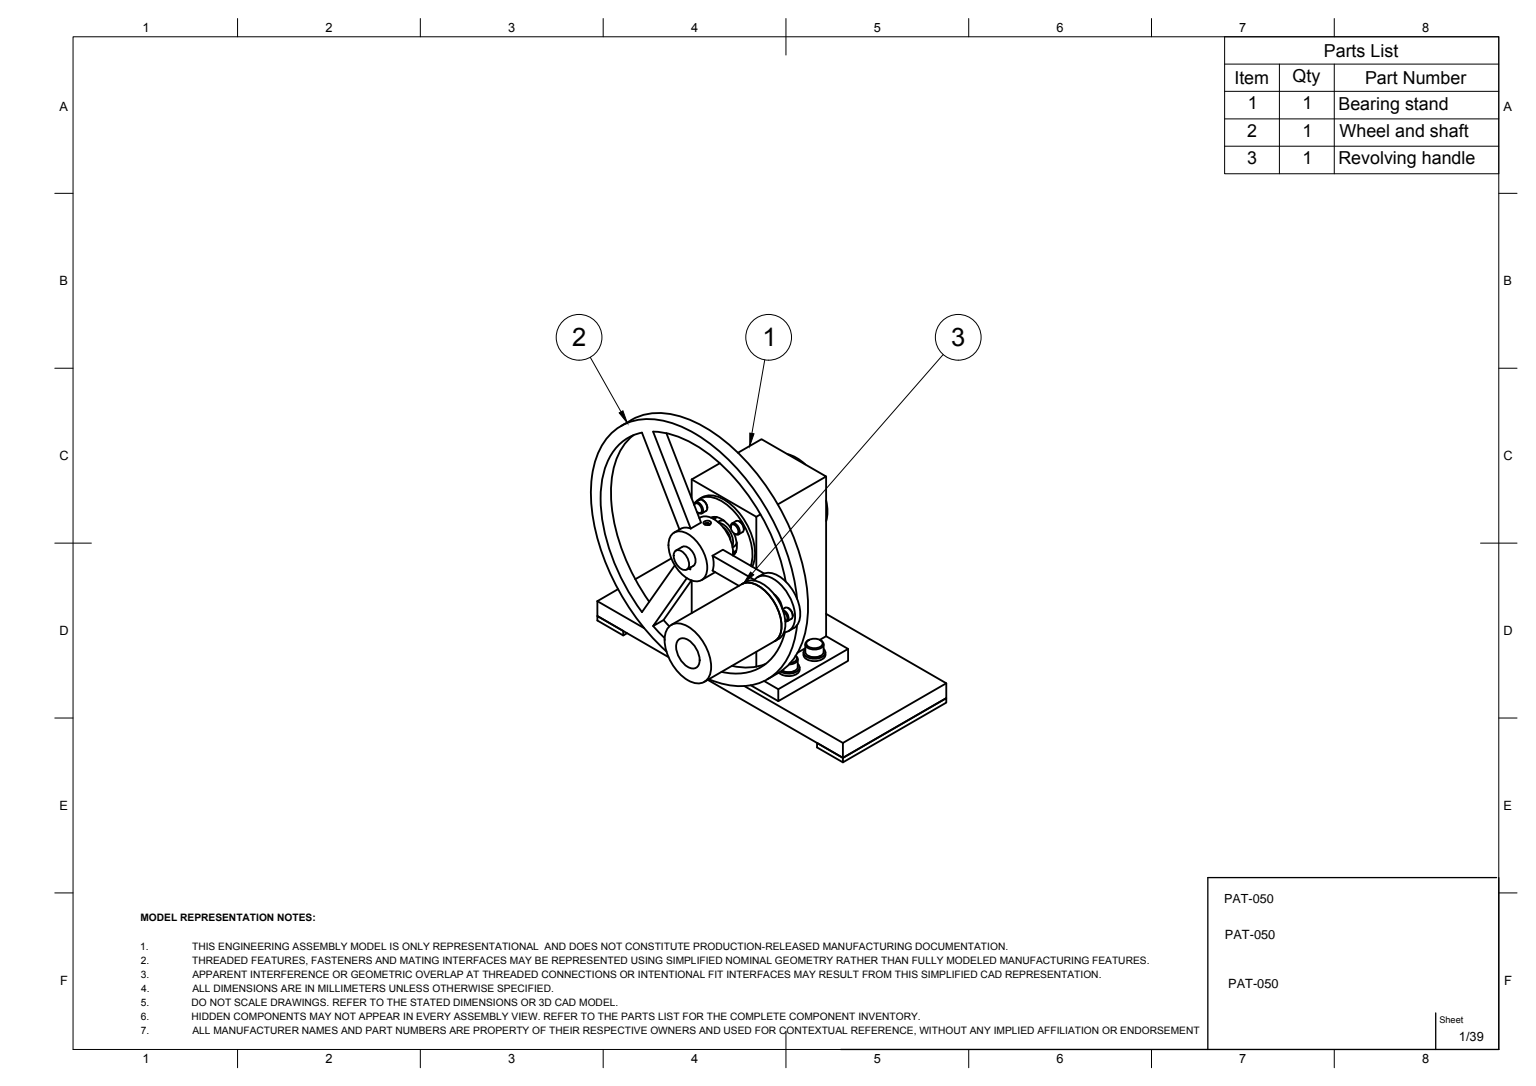
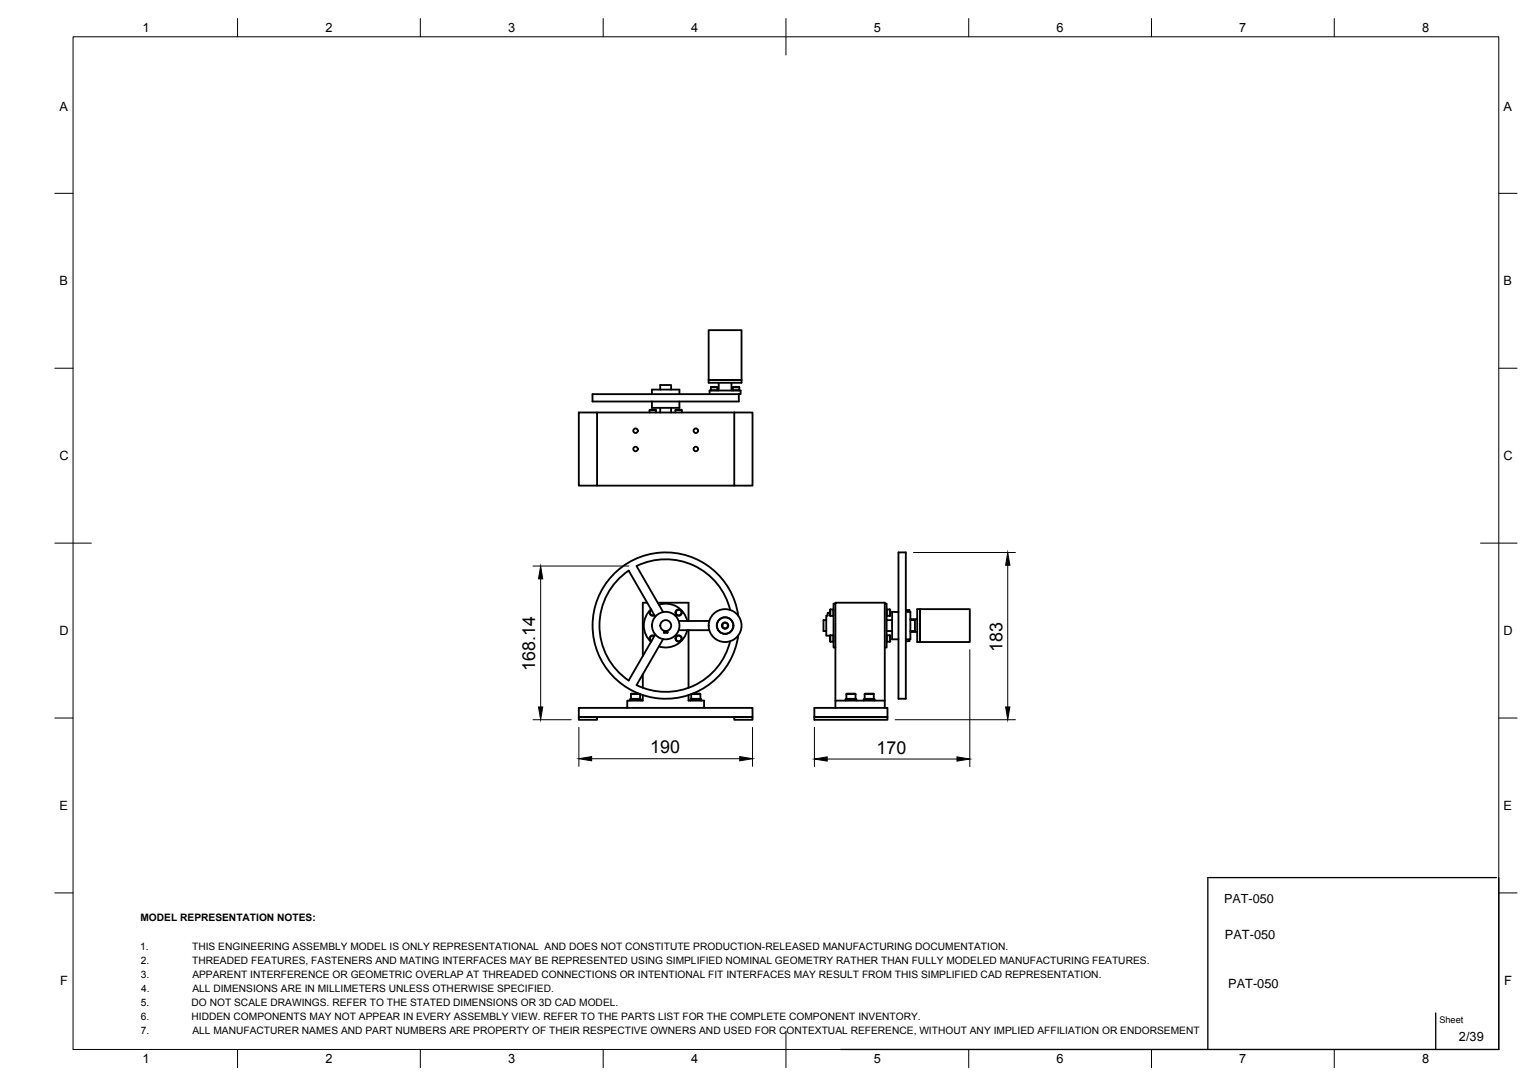
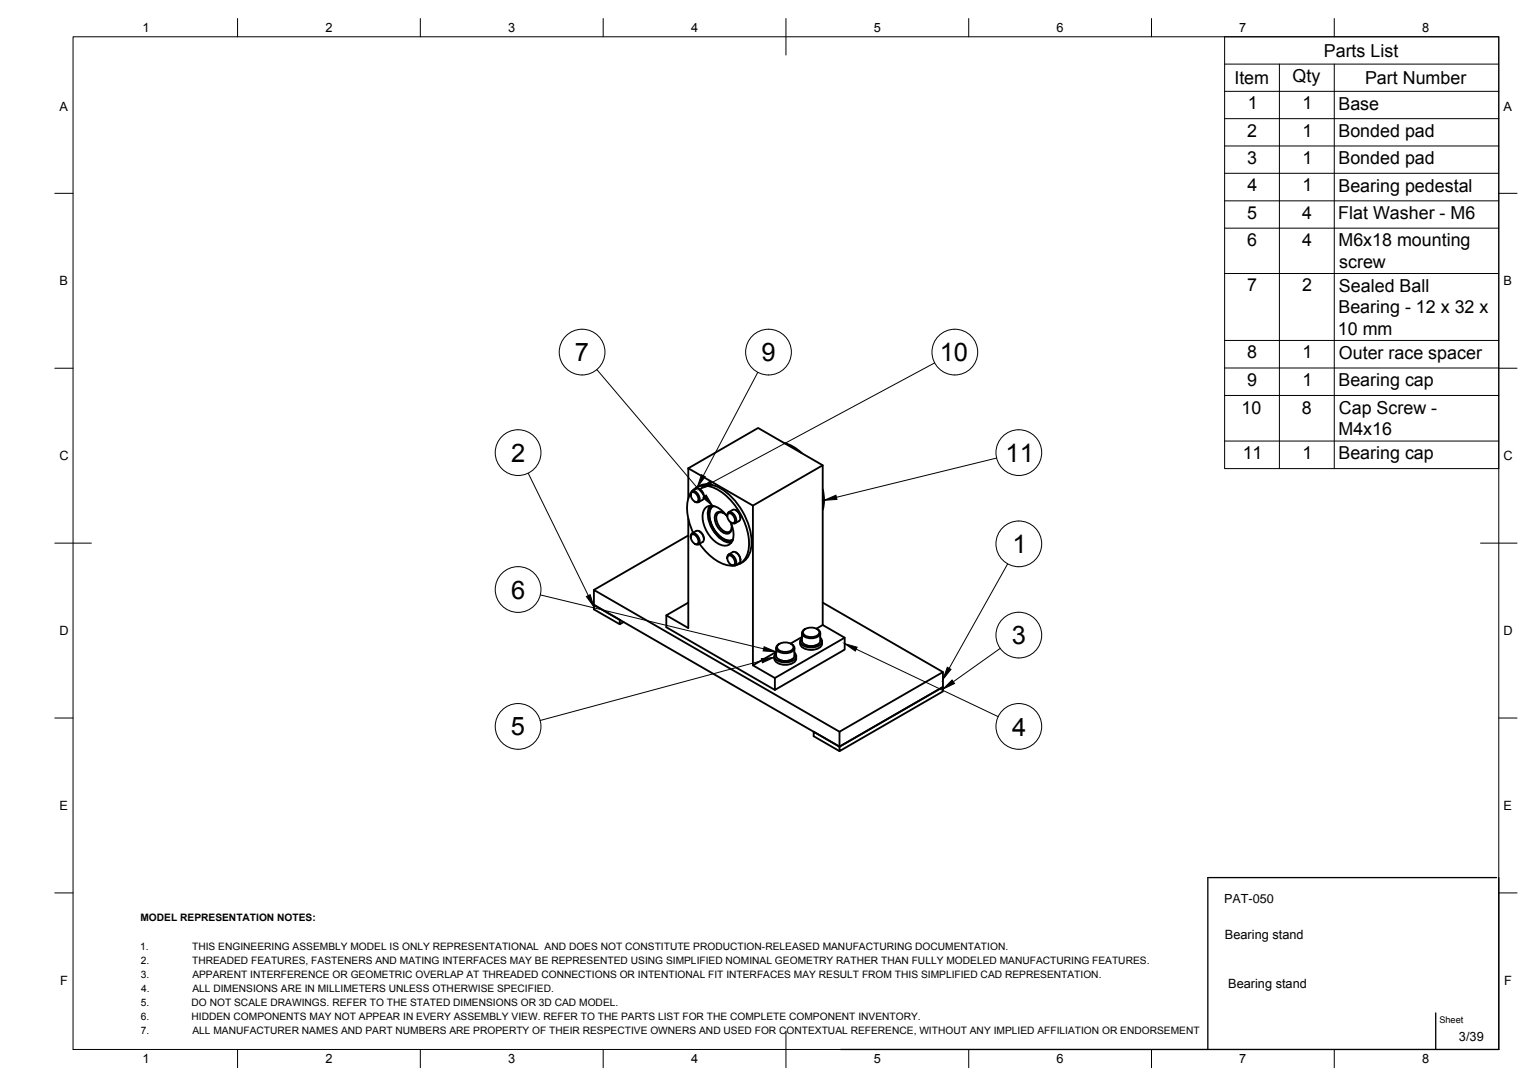
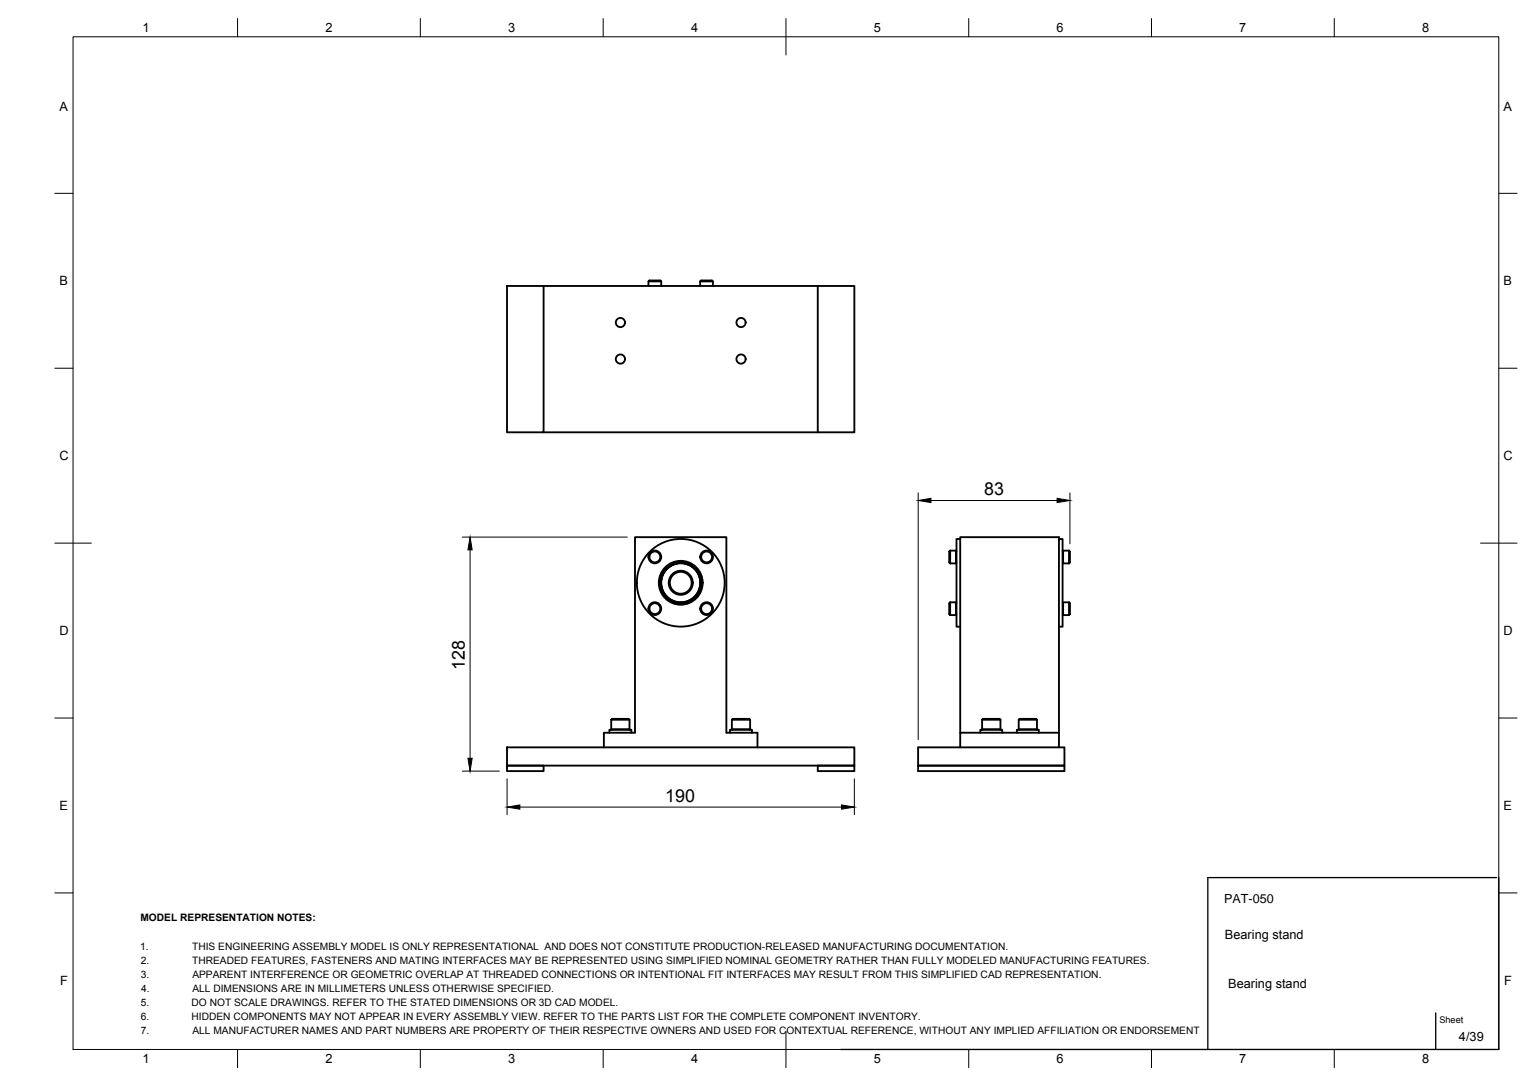
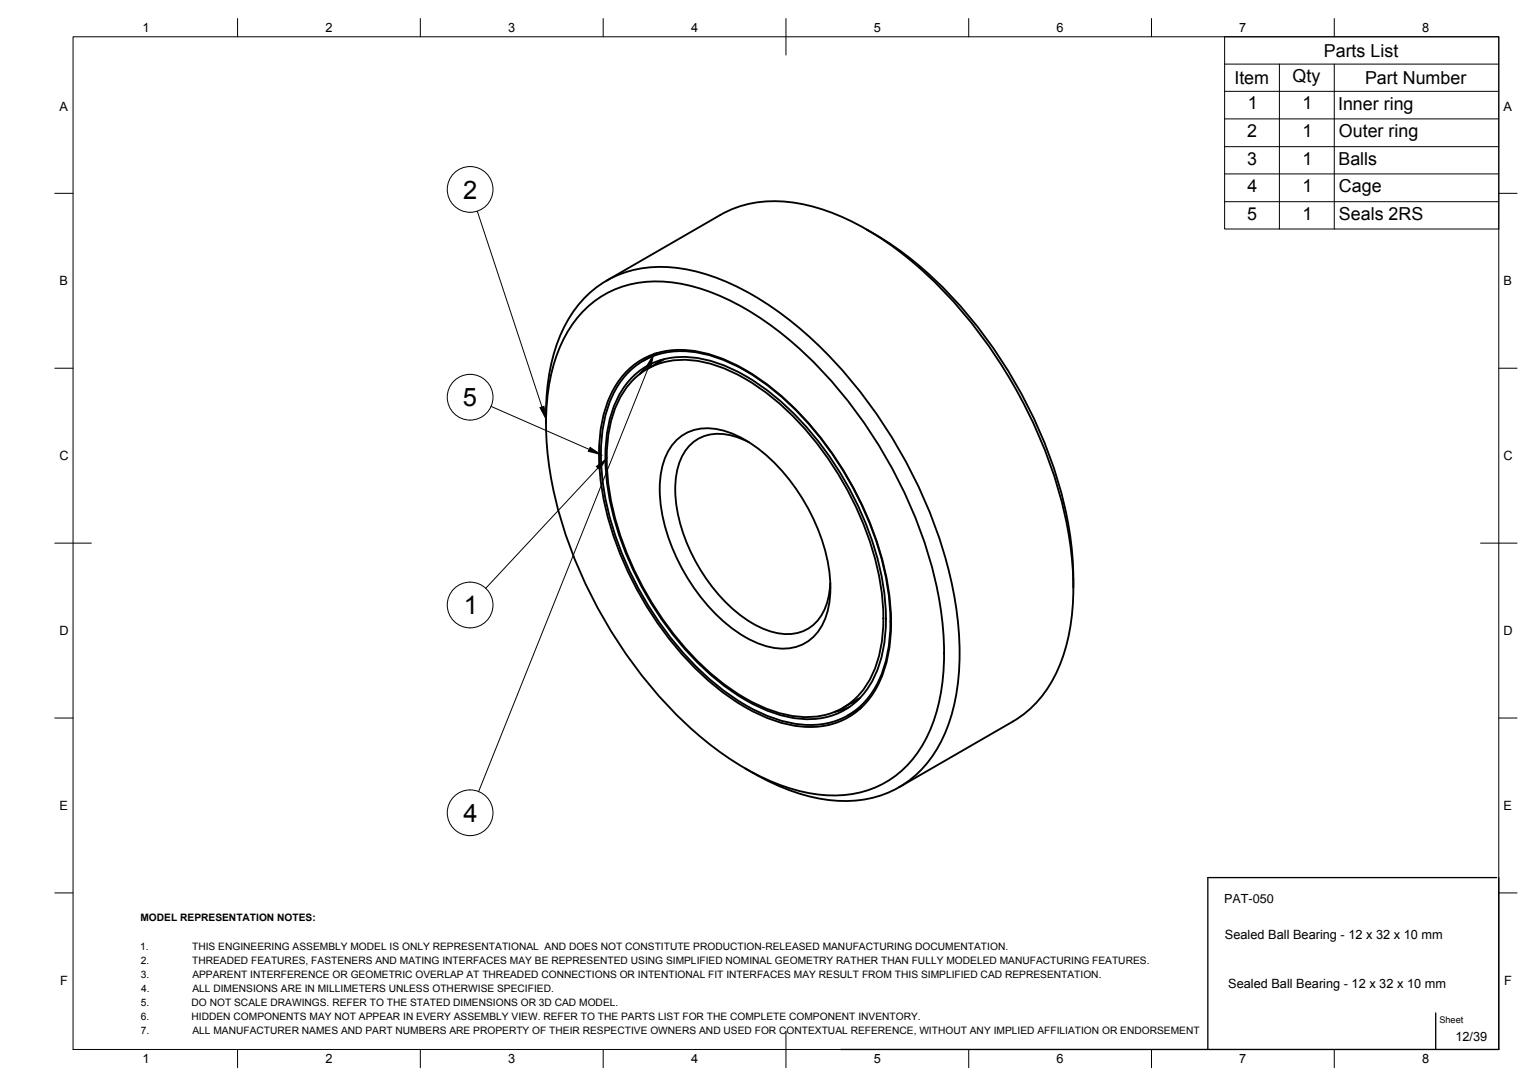
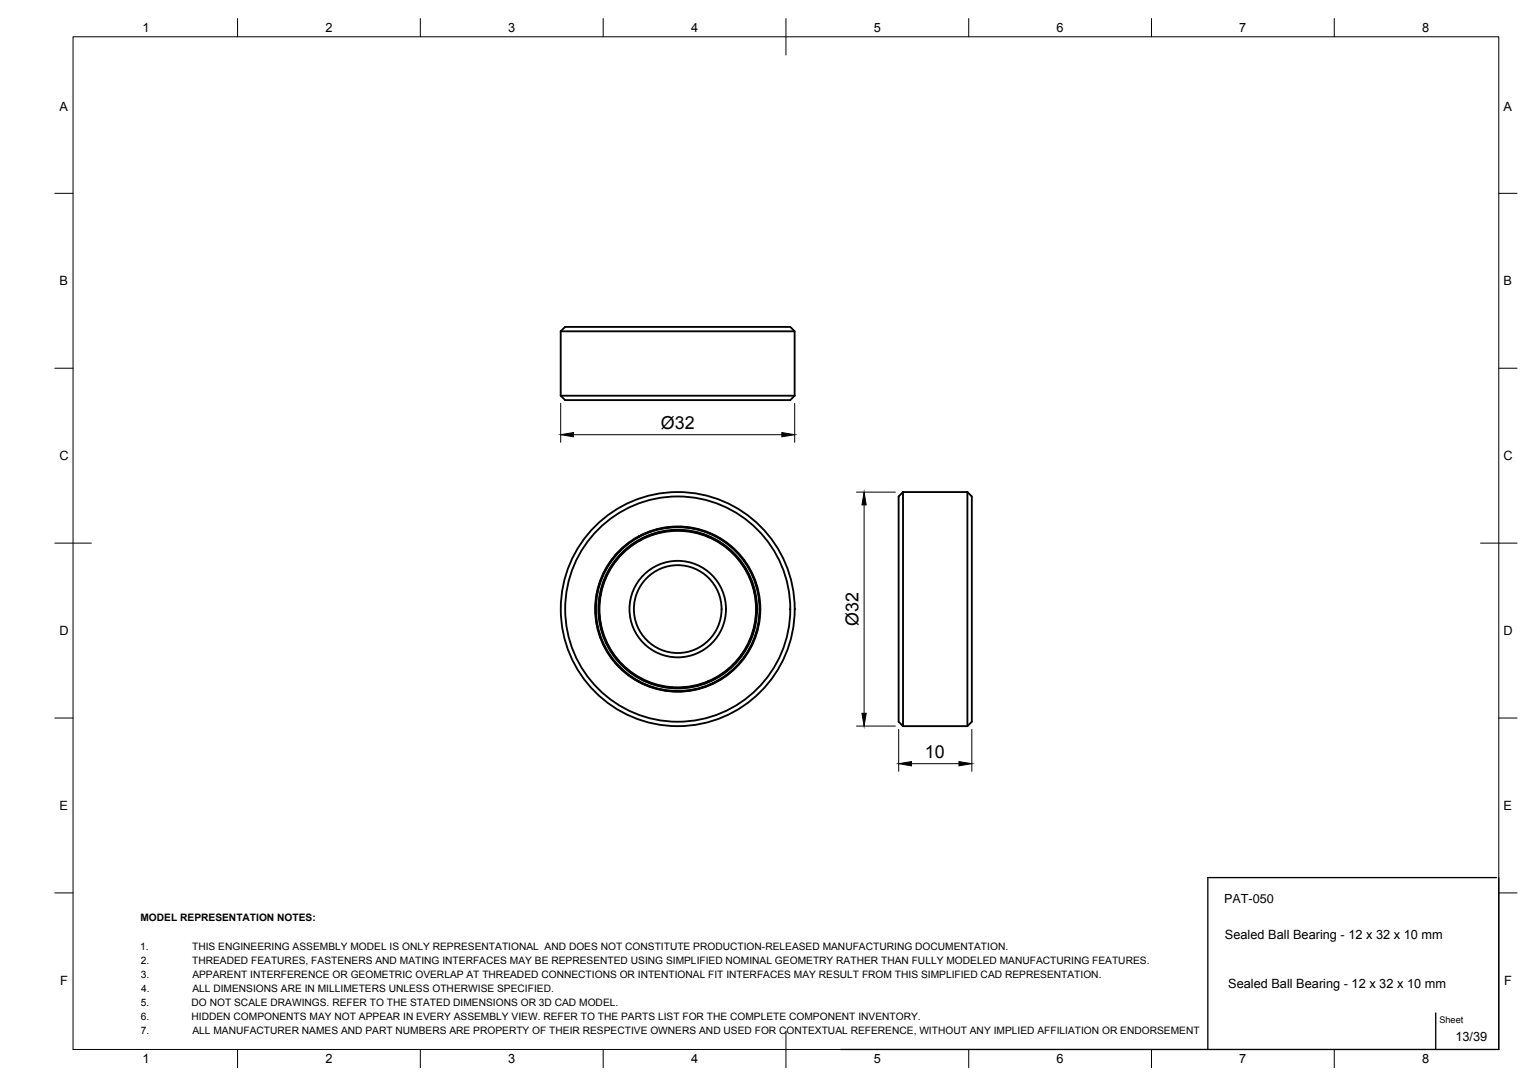
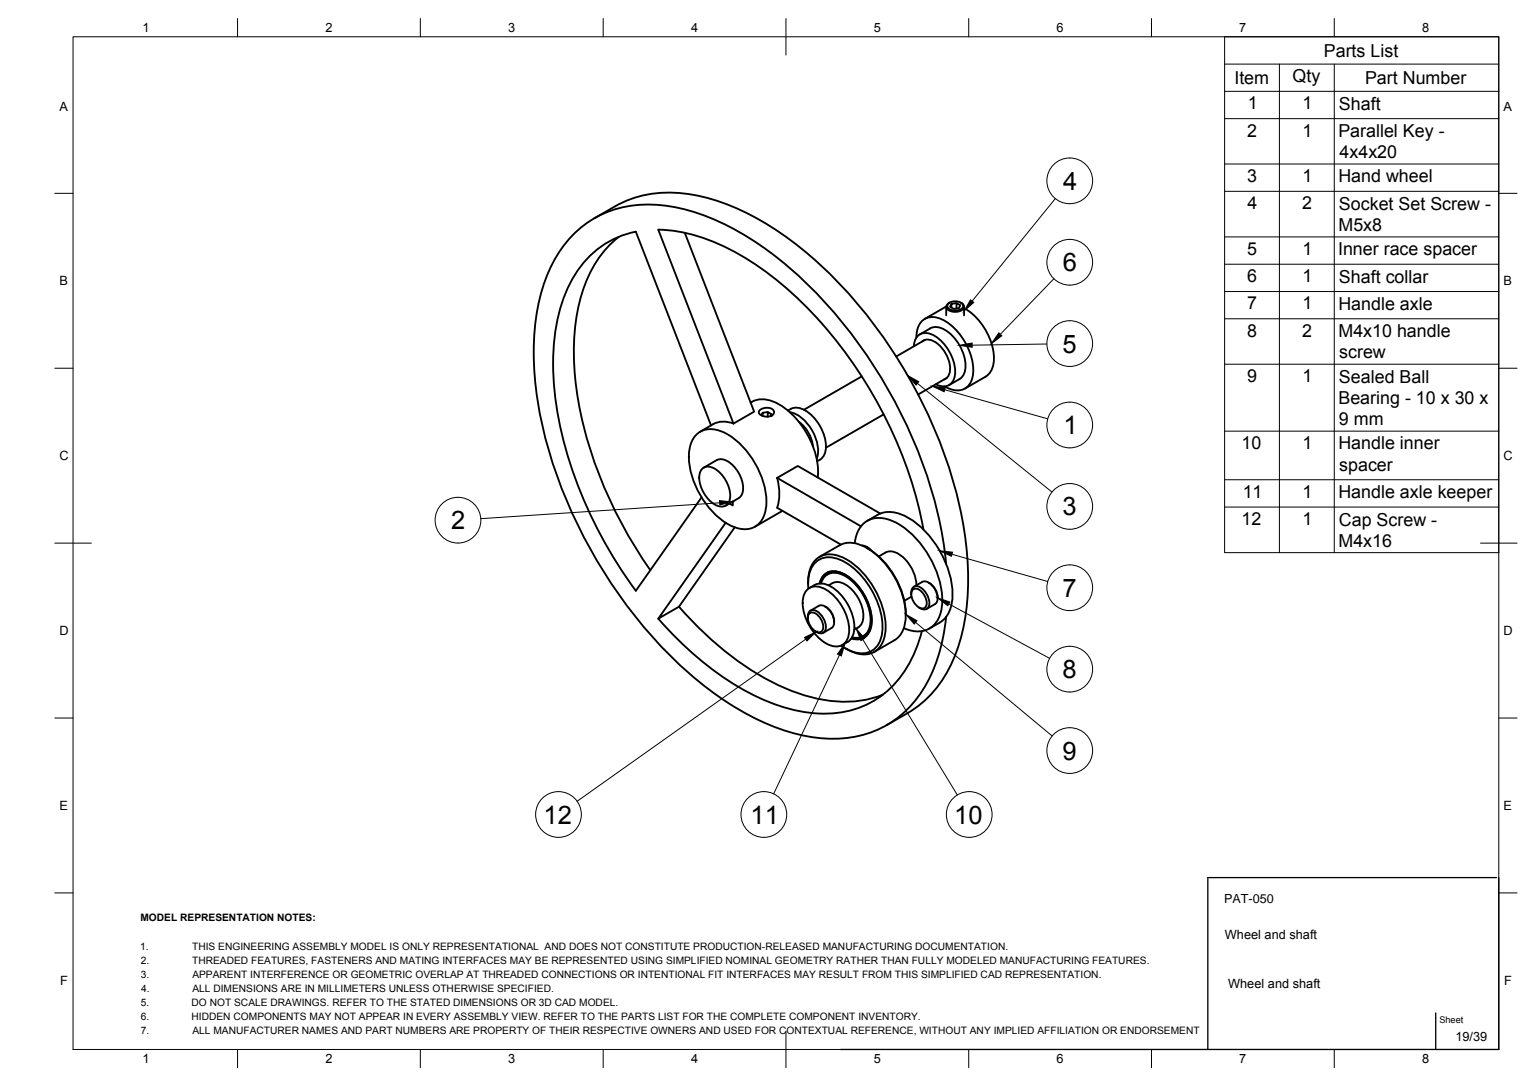
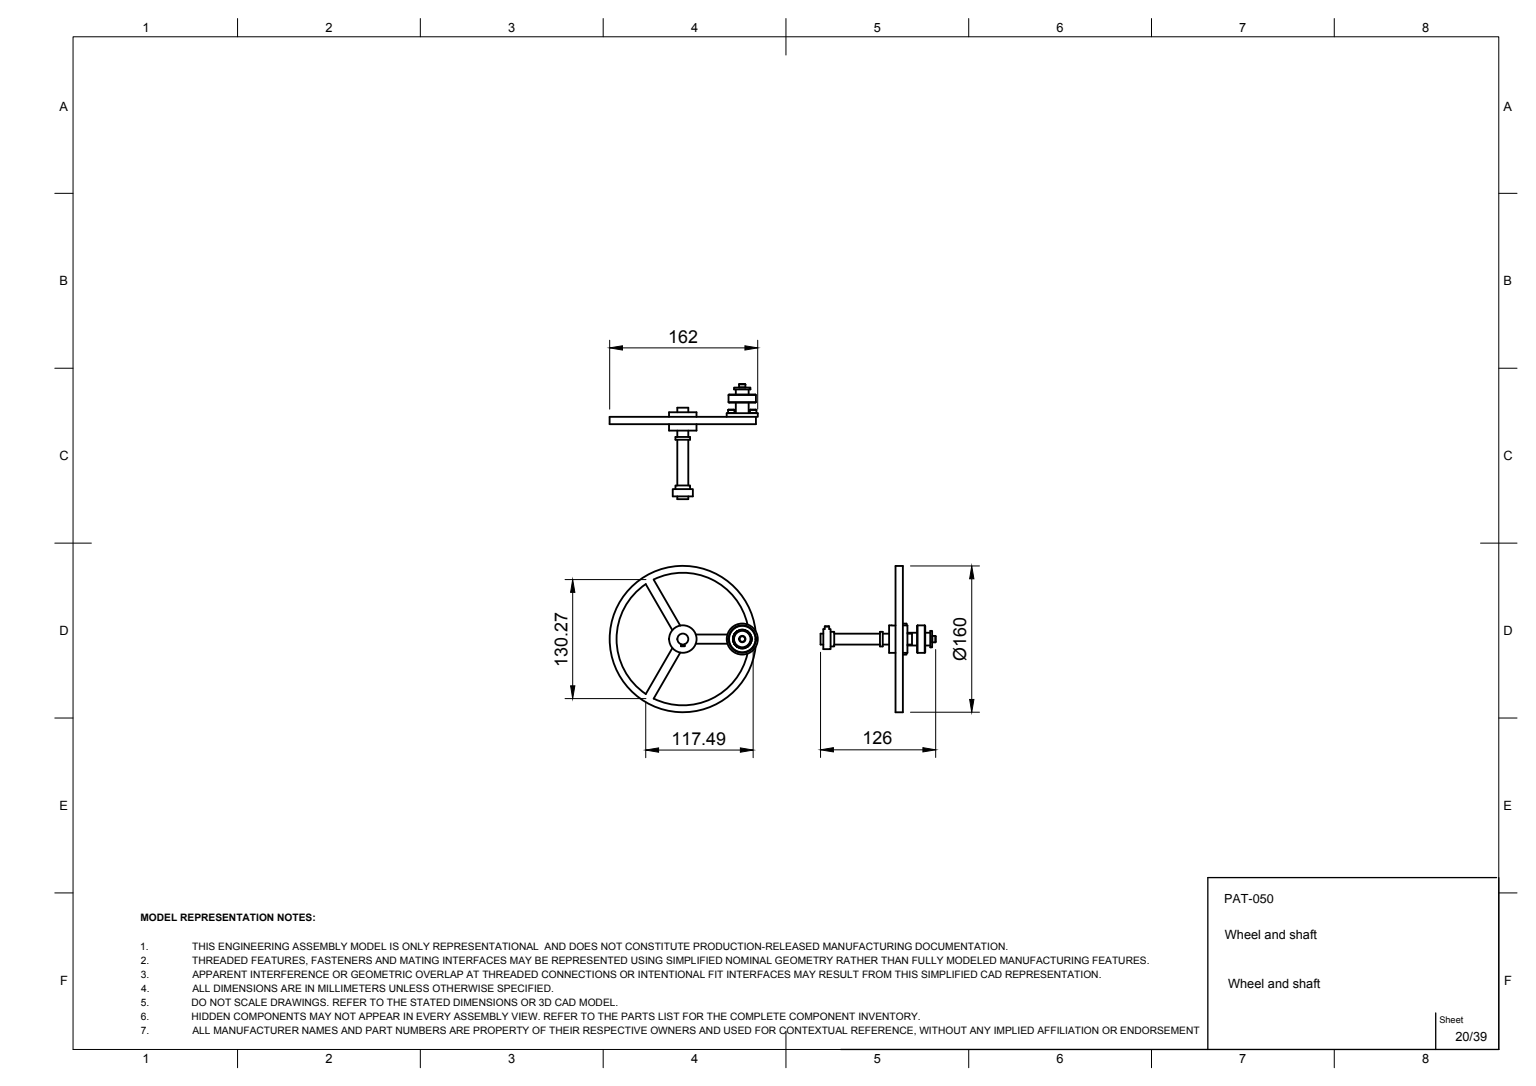
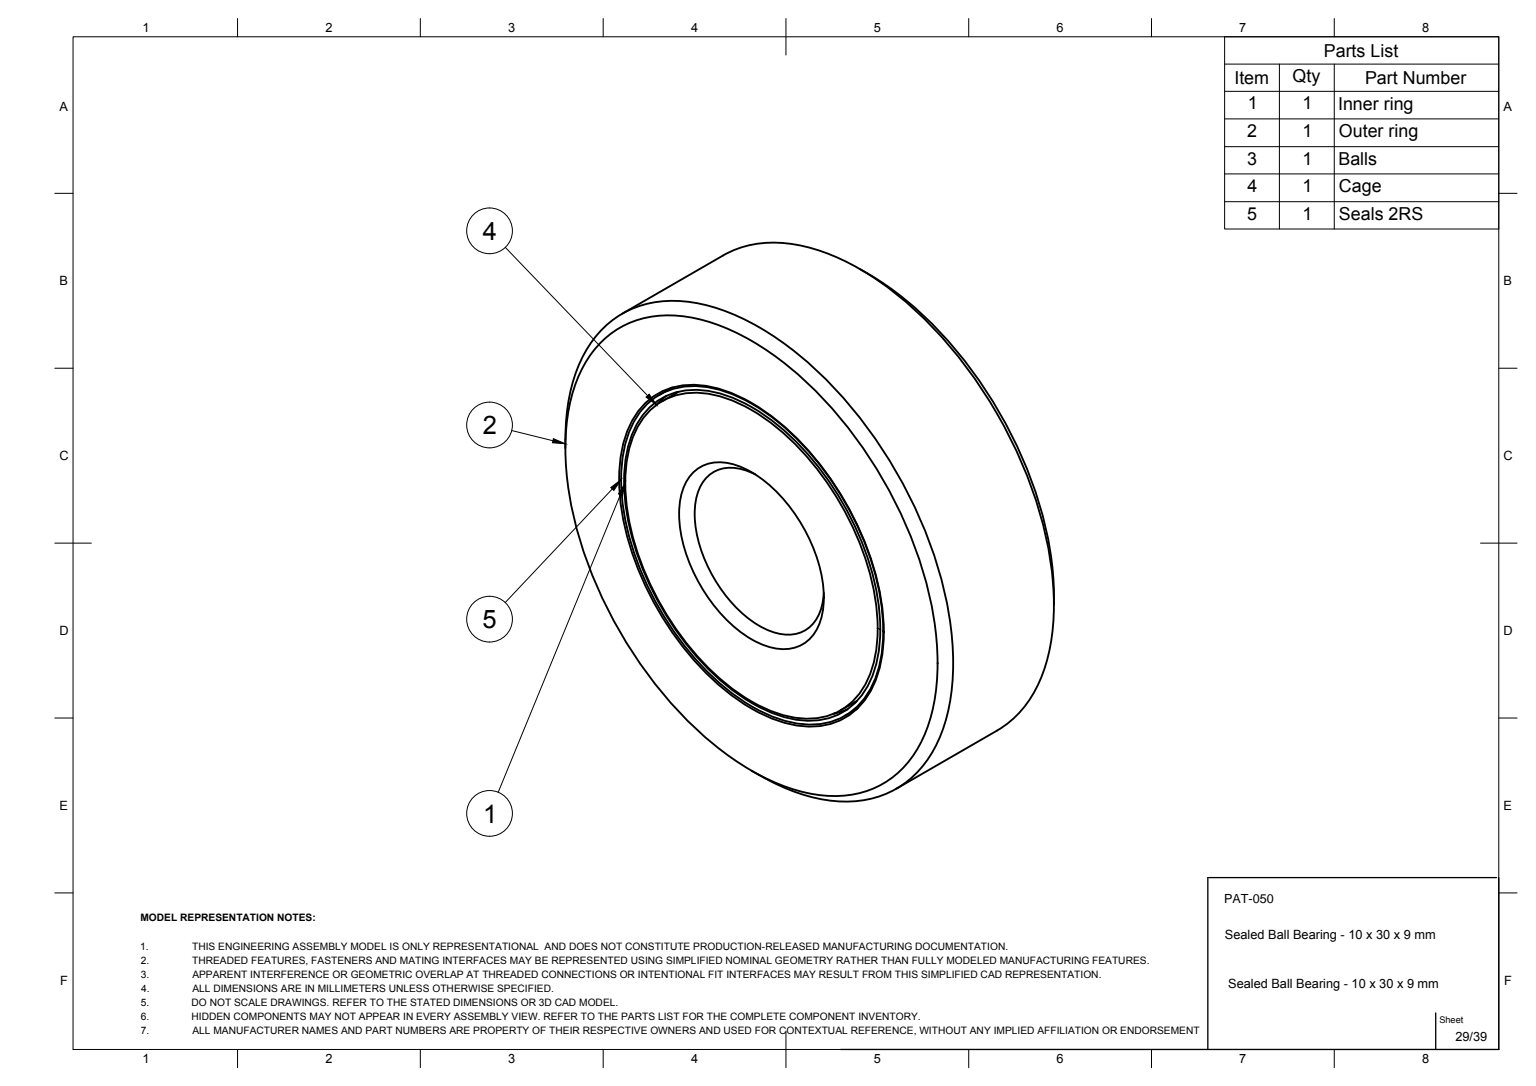
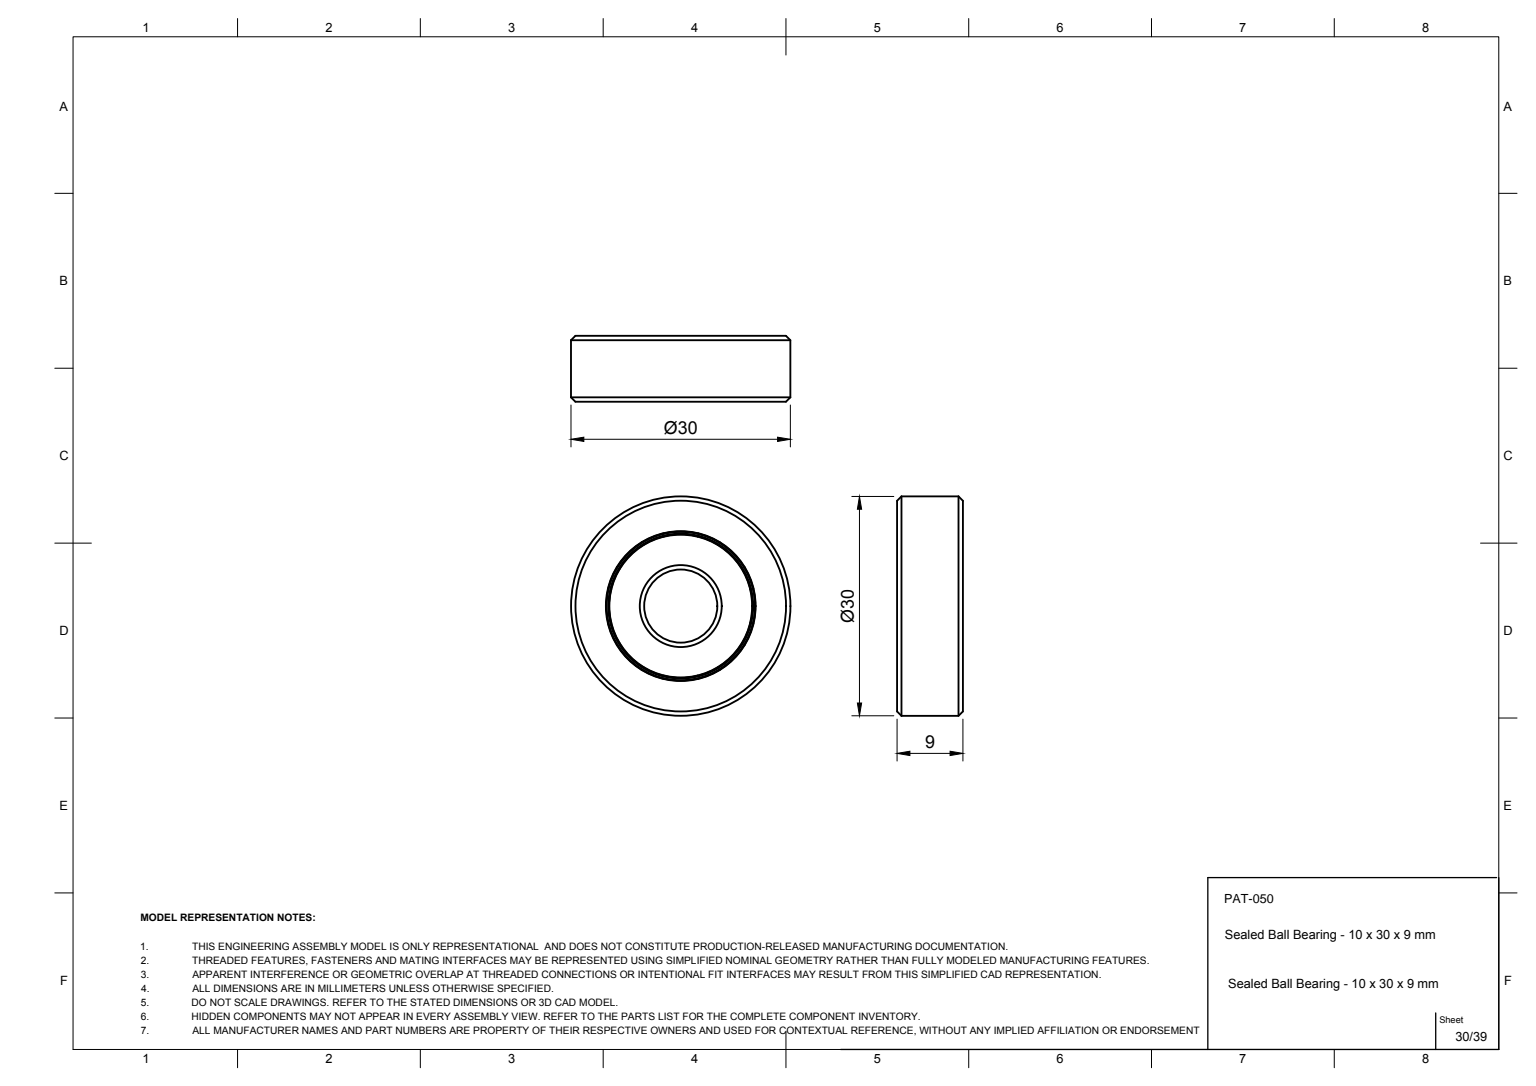
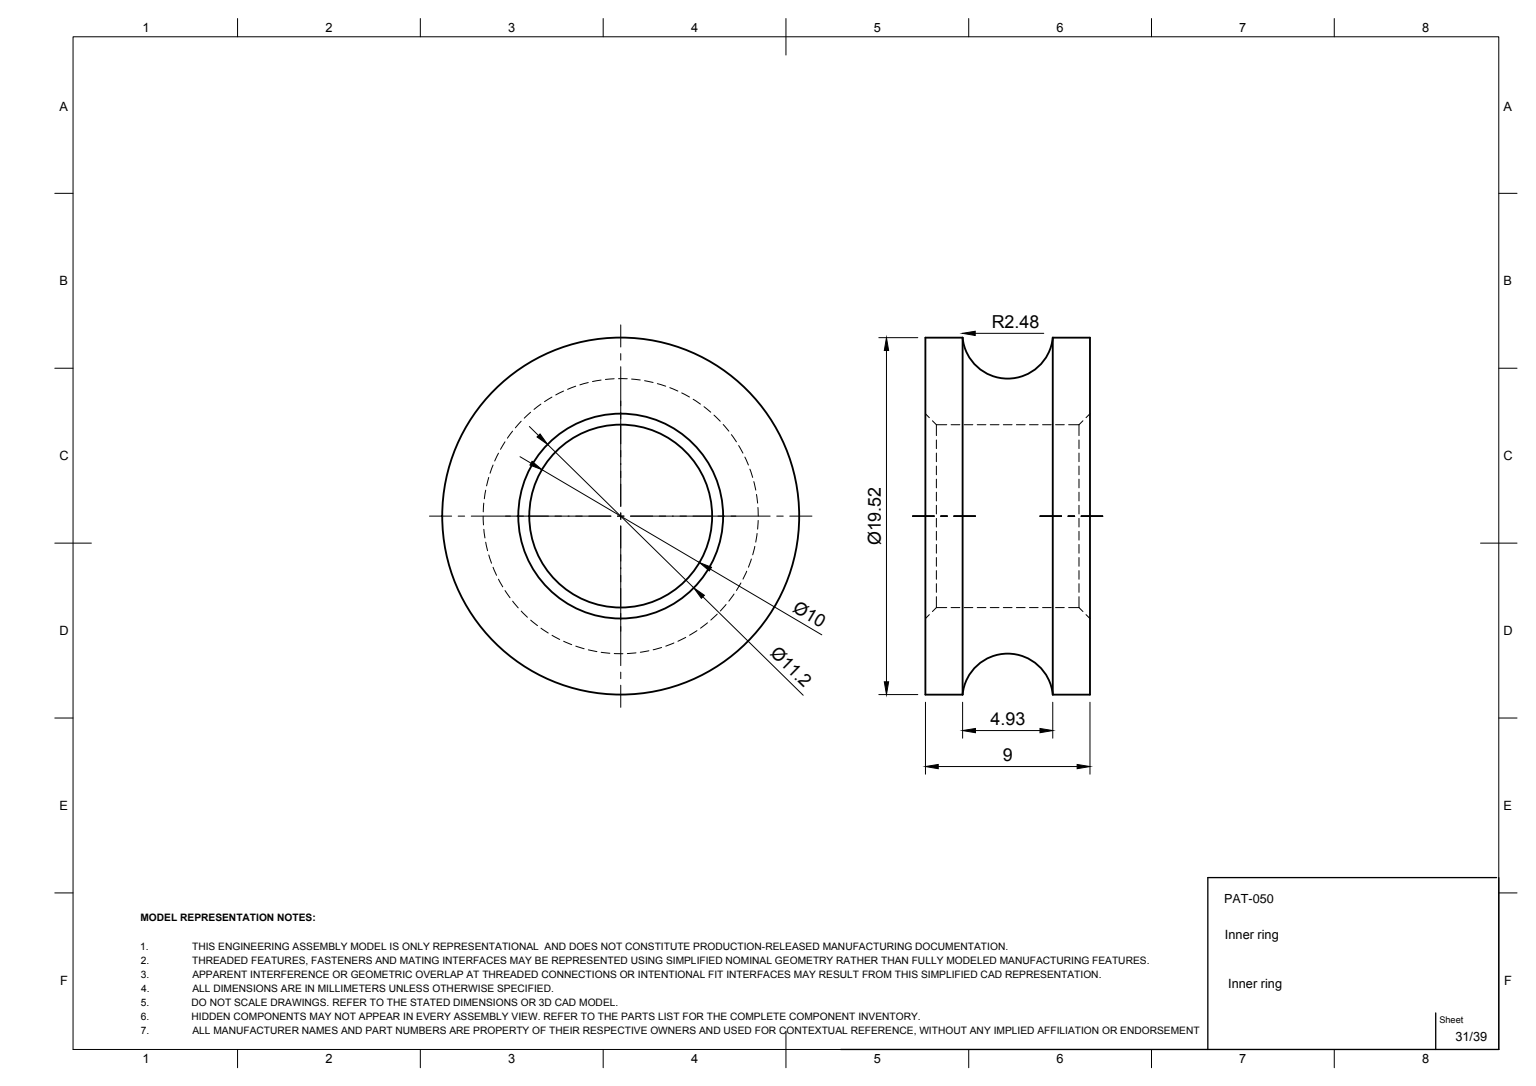
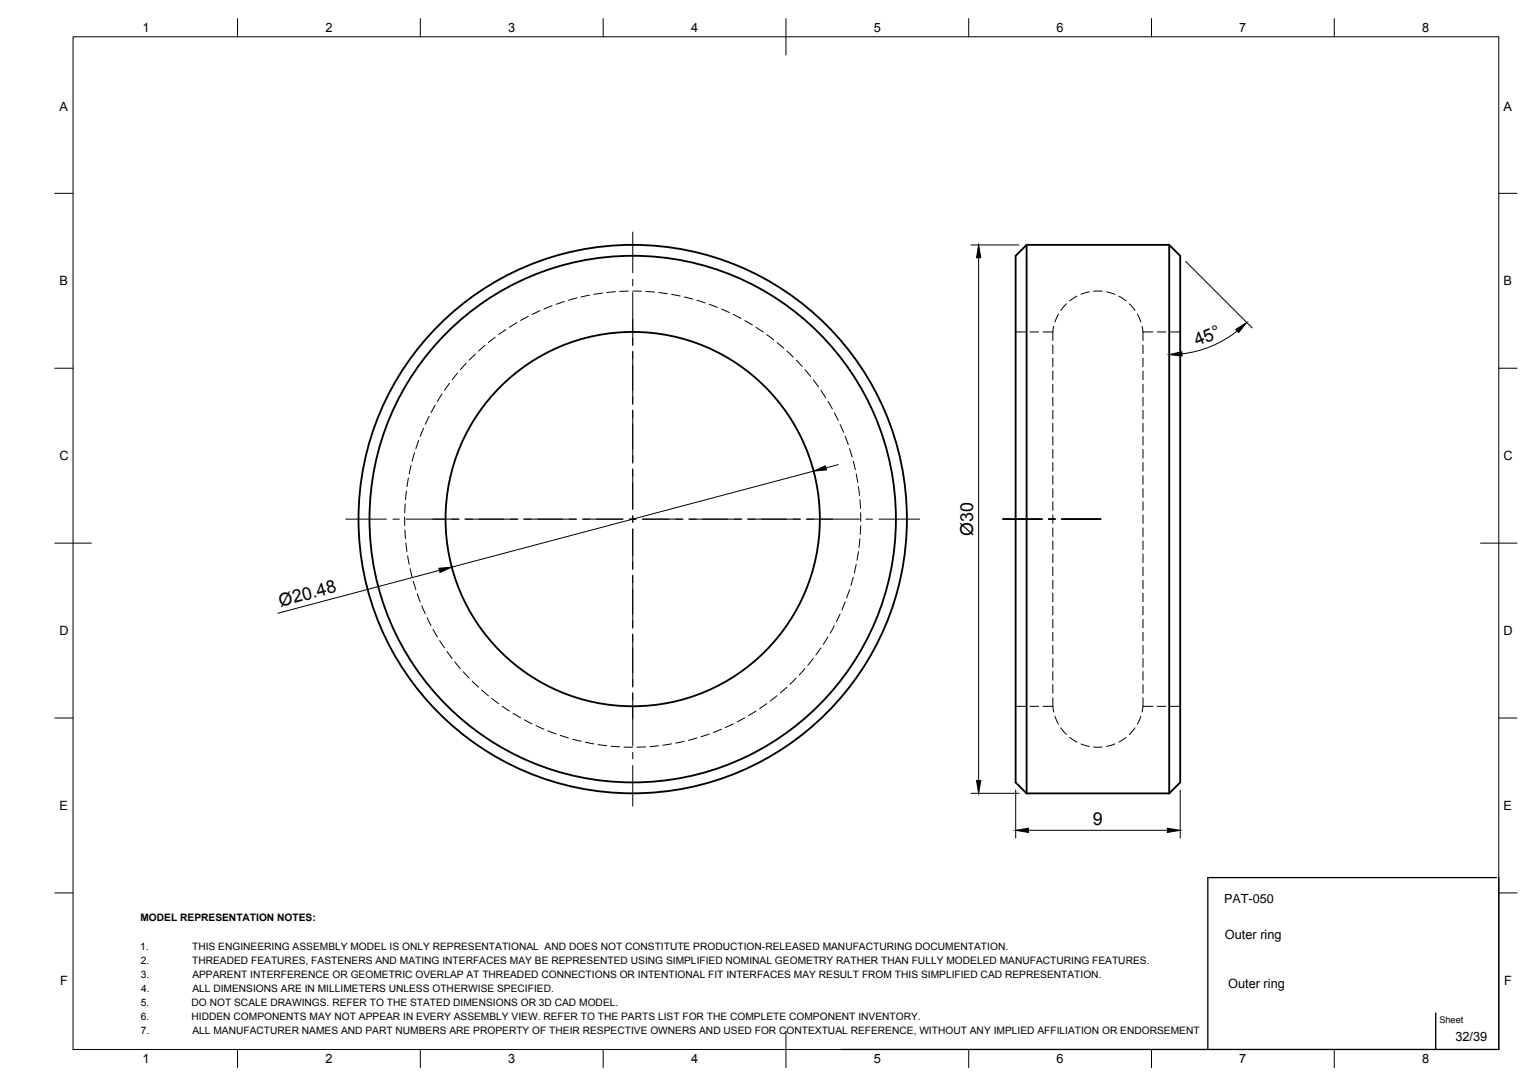
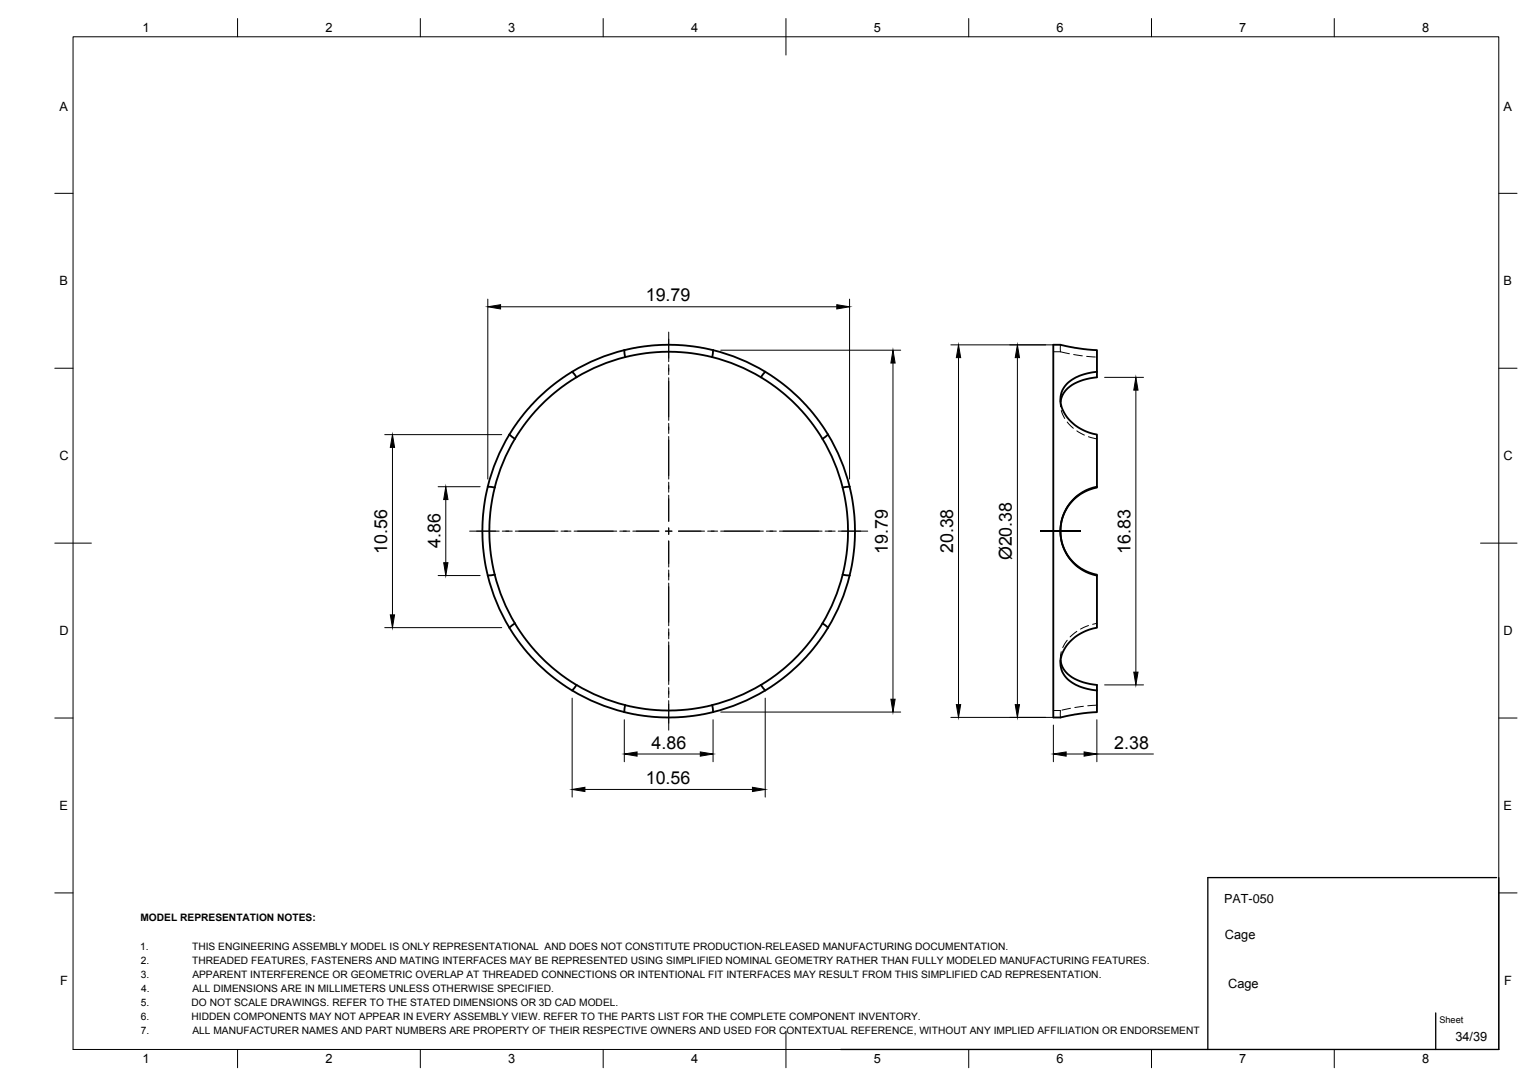
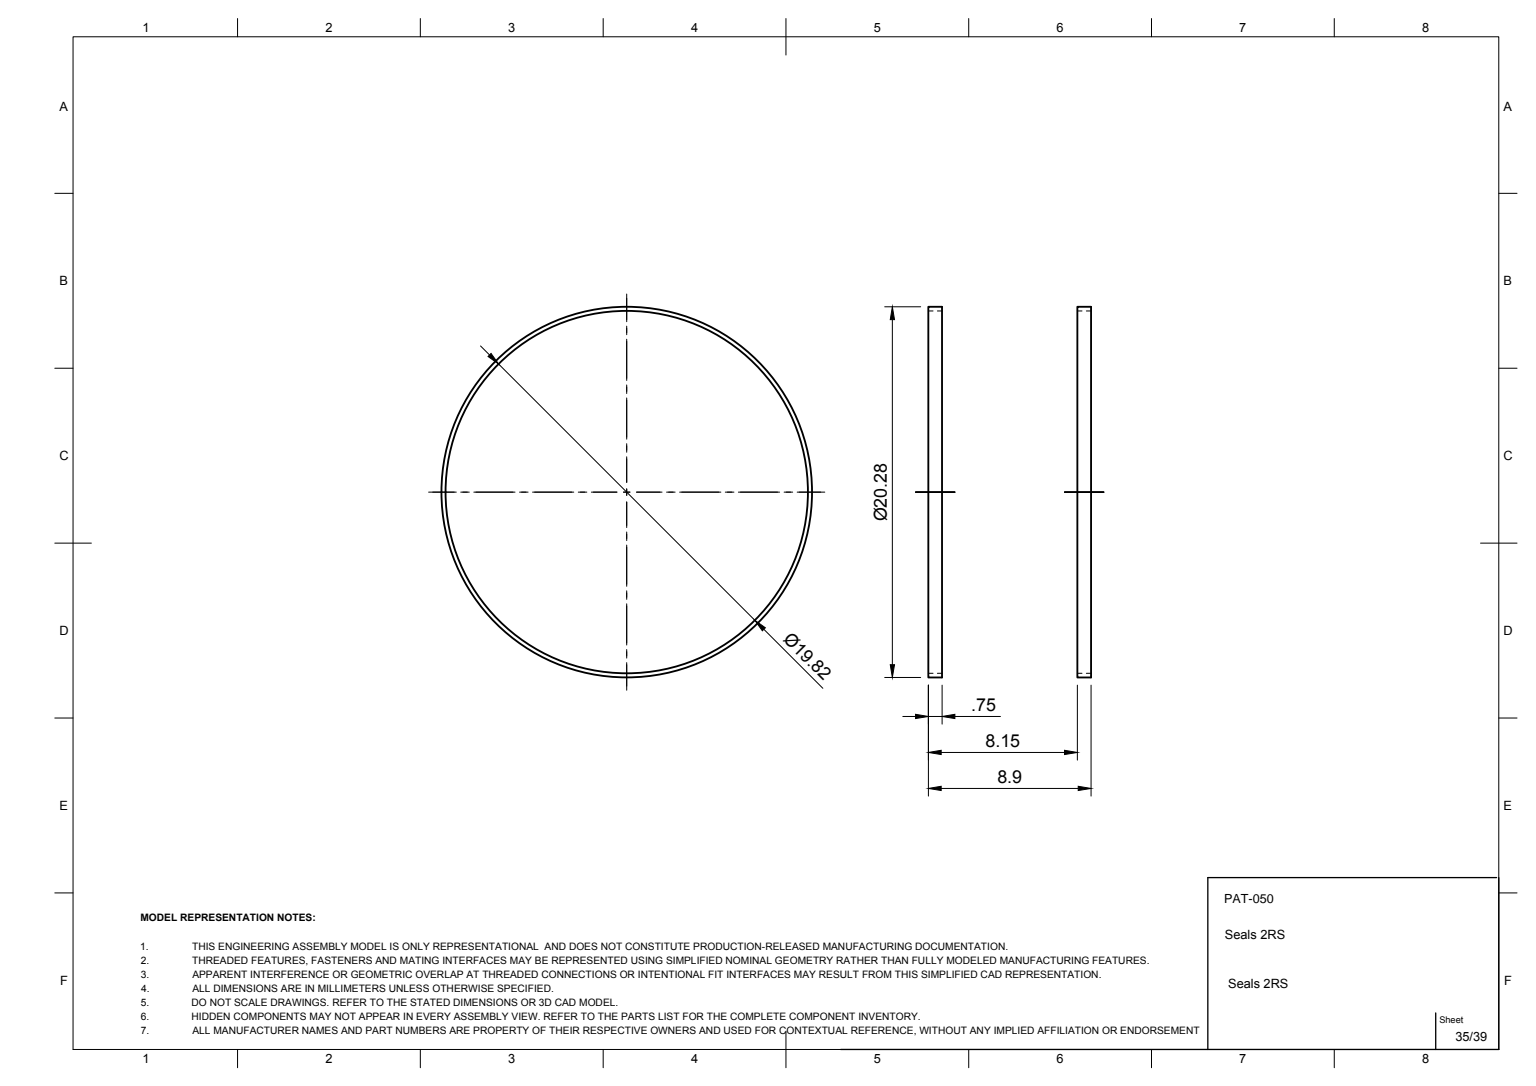
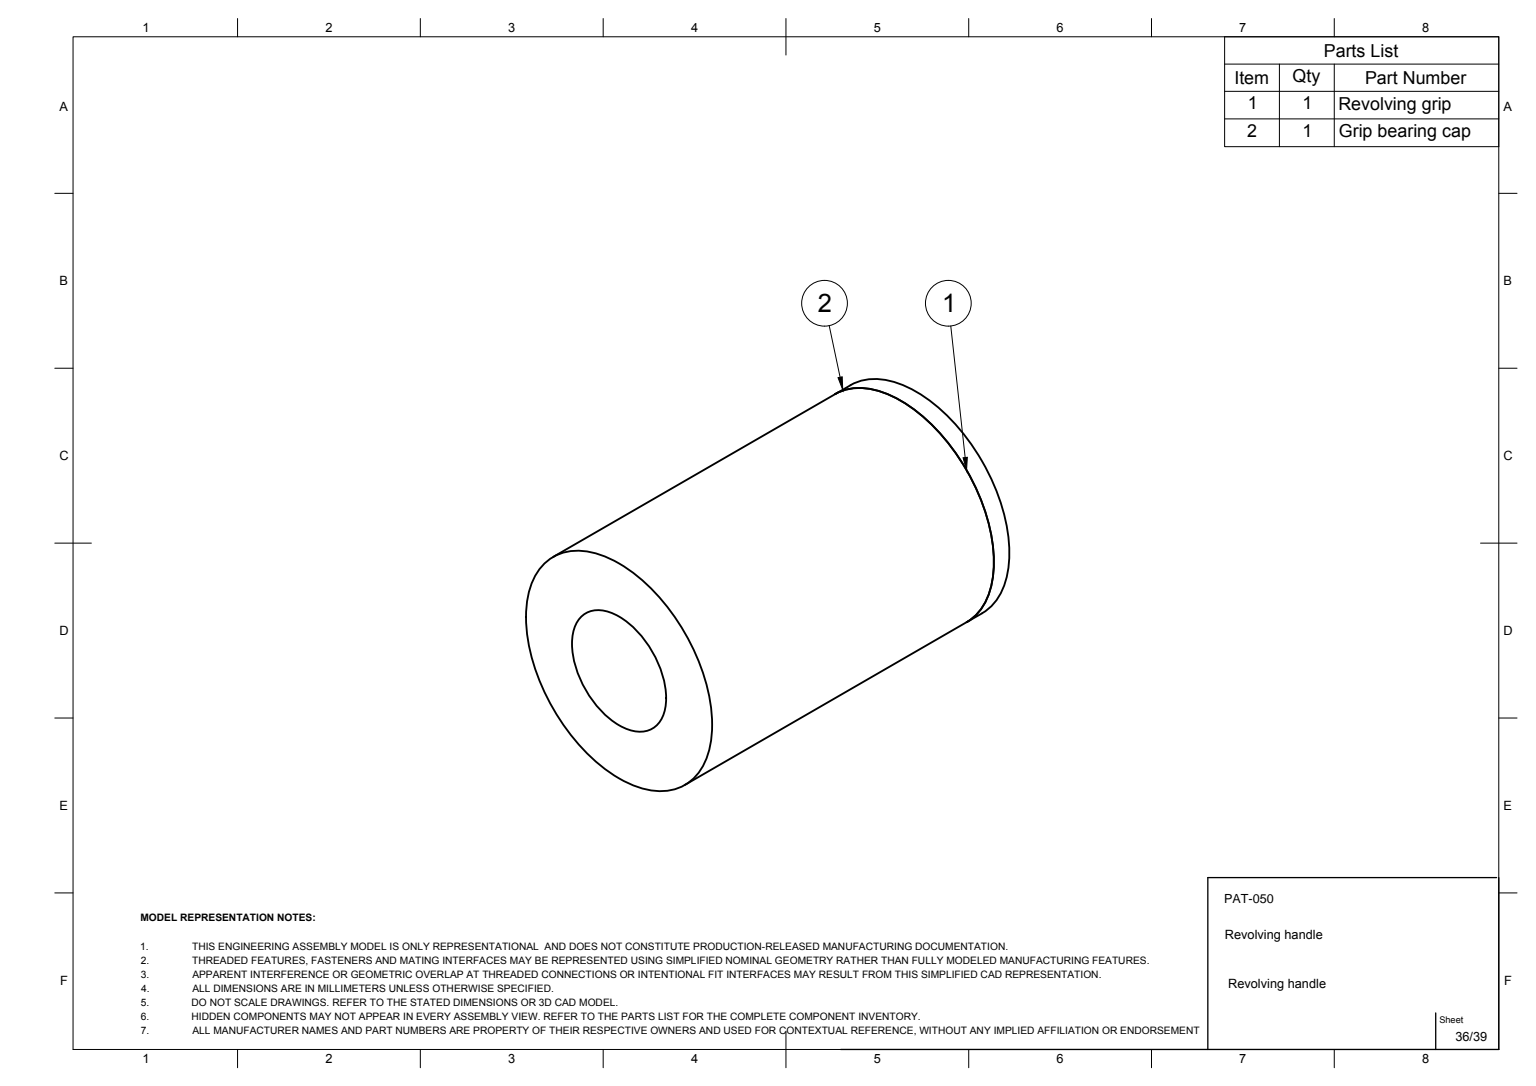
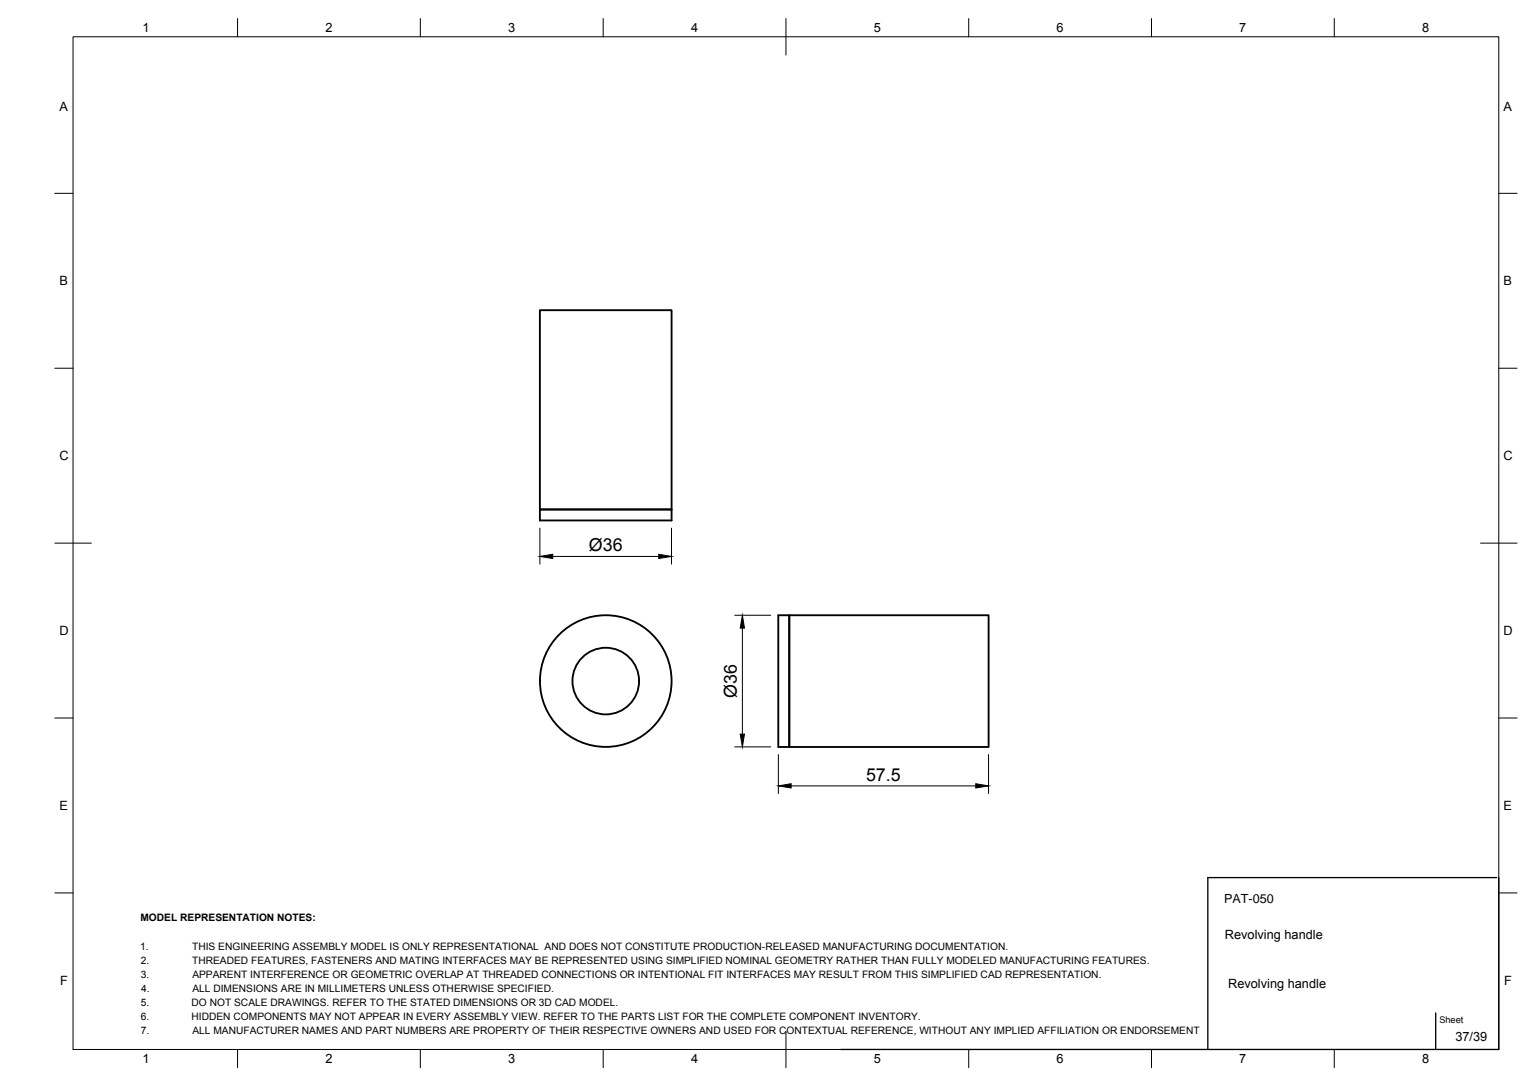
ISO-10303-21;
HEADER;
/* Generated by software containing ST-Developer
 * from STEP Tools, Inc. (www.steptools.com) 
 */

FILE_DESCRIPTION(
/* description */ ('Hand wheel with handle and shaft collar'),
/* implementation_level */ '2;1');

FILE_NAME(
/* name */ 'PAT-050',
/* time_stamp */ '2026-10-28T03:23:19-07:00',
/* author */ (''),
/* organization */ (''),
/* preprocessor_version */ 'ST-DEVELOPER v20.2',
/* originating_system */ 'Autodesk Translation Framework v15.17.0.0',
/* authorisation */ '');

FILE_SCHEMA (('AUTOMOTIVE_DESIGN { 1 0 10303 214 3 1 1 }'));
ENDSEC;

DATA;
#10=MECHANICAL_DESIGN_GEOMETRIC_PRESENTATION_REPRESENTATION('',(#395,#396,
#397,#398,#399,#400,#401,#402,#403,#404,#405,#406,#407,#408,#409,#410,#411,
#412,#413,#414,#415,#416,#417,#418,#419,#420,#421,#422,#423,#424,#425,#426,
#427,#428,#429,#430,#431,#432,#433,#434,#435,#436,#437,#438,#439,#440,#441),
#10510);
#11=ITEM_DEFINED_TRANSFORMATION($,$,#5863,#5985);
#12=ITEM_DEFINED_TRANSFORMATION($,$,#5883,#5986);
#13=ITEM_DEFINED_TRANSFORMATION($,$,#5903,#5987);
#14=ITEM_DEFINED_TRANSFORMATION($,$,#5918,#5988);
#15=ITEM_DEFINED_TRANSFORMATION($,$,#5968,#5989);
#16=ITEM_DEFINED_TRANSFORMATION($,$,#6193,#6321);
#17=ITEM_DEFINED_TRANSFORMATION($,$,#6213,#6322);
#18=ITEM_DEFINED_TRANSFORMATION($,$,#6233,#6323);
#19=ITEM_DEFINED_TRANSFORMATION($,$,#6250,#6324);
#20=ITEM_DEFINED_TRANSFORMATION($,$,#6304,#6325);
#21=ITEM_DEFINED_TRANSFORMATION($,$,#5699,#6352);
#22=ITEM_DEFINED_TRANSFORMATION($,$,#5718,#6353);
#23=ITEM_DEFINED_TRANSFORMATION($,$,#5725,#6354);
#24=ITEM_DEFINED_TRANSFORMATION($,$,#5732,#6355);
#25=ITEM_DEFINED_TRANSFORMATION($,$,#5770,#6356);
#26=ITEM_DEFINED_TRANSFORMATION($,$,#5779,#6357);
#27=ITEM_DEFINED_TRANSFORMATION($,$,#5804,#6358);
#28=ITEM_DEFINED_TRANSFORMATION($,$,#5829,#6359);
#29=ITEM_DEFINED_TRANSFORMATION($,$,#5838,#6360);
#30=ITEM_DEFINED_TRANSFORMATION($,$,#5829,#6361);
#31=ITEM_DEFINED_TRANSFORMATION($,$,#5838,#6362);
#32=ITEM_DEFINED_TRANSFORMATION($,$,#5829,#6363);
#33=ITEM_DEFINED_TRANSFORMATION($,$,#5838,#6364);
#34=ITEM_DEFINED_TRANSFORMATION($,$,#5829,#6365);
#35=ITEM_DEFINED_TRANSFORMATION($,$,#5838,#6366);
#36=ITEM_DEFINED_TRANSFORMATION($,$,#5862,#6367);
#37=ITEM_DEFINED_TRANSFORMATION($,$,#5862,#6368);
#38=ITEM_DEFINED_TRANSFORMATION($,$,#6326,#6369);
#39=ITEM_DEFINED_TRANSFORMATION($,$,#6326,#6370);
#40=ITEM_DEFINED_TRANSFORMATION($,$,#6326,#6371);
#41=ITEM_DEFINED_TRANSFORMATION($,$,#6326,#6372);
#42=ITEM_DEFINED_TRANSFORMATION($,$,#6326,#6373);
#43=ITEM_DEFINED_TRANSFORMATION($,$,#6326,#6374);
#44=ITEM_DEFINED_TRANSFORMATION($,$,#6326,#6375);
#45=ITEM_DEFINED_TRANSFORMATION($,$,#6326,#6376);
#46=ITEM_DEFINED_TRANSFORMATION($,$,#5991,#6377);
#47=ITEM_DEFINED_TRANSFORMATION($,$,#6012,#6378);
#48=ITEM_DEFINED_TRANSFORMATION($,$,#6062,#6379);
#49=ITEM_DEFINED_TRANSFORMATION($,$,#6071,#6380);
#50=ITEM_DEFINED_TRANSFORMATION($,$,#6086,#6381);
#51=ITEM_DEFINED_TRANSFORMATION($,$,#6110,#6382);
#52=ITEM_DEFINED_TRANSFORMATION($,$,#6119,#6383);
#53=ITEM_DEFINED_TRANSFORMATION($,$,#6128,#6384);
#54=ITEM_DEFINED_TRANSFORMATION($,$,#6151,#6385);
#55=ITEM_DEFINED_TRANSFORMATION($,$,#6151,#6386);
#56=ITEM_DEFINED_TRANSFORMATION($,$,#6168,#6387);
#57=ITEM_DEFINED_TRANSFORMATION($,$,#6168,#6388);
#58=ITEM_DEFINED_TRANSFORMATION($,$,#6192,#6389);
#59=ITEM_DEFINED_TRANSFORMATION($,$,#6326,#6390);
#60=ITEM_DEFINED_TRANSFORMATION($,$,#6392,#6414);
#61=ITEM_DEFINED_TRANSFORMATION($,$,#6405,#6415);
#62=ITEM_DEFINED_TRANSFORMATION($,$,#5698,#6416);
#63=ITEM_DEFINED_TRANSFORMATION($,$,#5990,#6417);
#64=ITEM_DEFINED_TRANSFORMATION($,$,#6391,#6418);
#65=(
REPRESENTATION_RELATIONSHIP($,$,#10657,#10656)
REPRESENTATION_RELATIONSHIP_WITH_TRANSFORMATION(#11)
SHAPE_REPRESENTATION_RELATIONSHIP()
);
#66=(
REPRESENTATION_RELATIONSHIP($,$,#10658,#10656)
REPRESENTATION_RELATIONSHIP_WITH_TRANSFORMATION(#12)
SHAPE_REPRESENTATION_RELATIONSHIP()
);
#67=(
REPRESENTATION_RELATIONSHIP($,$,#10659,#10656)
REPRESENTATION_RELATIONSHIP_WITH_TRANSFORMATION(#13)
SHAPE_REPRESENTATION_RELATIONSHIP()
);
#68=(
REPRESENTATION_RELATIONSHIP($,$,#10660,#10656)
REPRESENTATION_RELATIONSHIP_WITH_TRANSFORMATION(#14)
SHAPE_REPRESENTATION_RELATIONSHIP()
);
#69=(
REPRESENTATION_RELATIONSHIP($,$,#10661,#10656)
REPRESENTATION_RELATIONSHIP_WITH_TRANSFORMATION(#15)
SHAPE_REPRESENTATION_RELATIONSHIP()
);
#70=(
REPRESENTATION_RELATIONSHIP($,$,#10674,#10673)
REPRESENTATION_RELATIONSHIP_WITH_TRANSFORMATION(#16)
SHAPE_REPRESENTATION_RELATIONSHIP()
);
#71=(
REPRESENTATION_RELATIONSHIP($,$,#10675,#10673)
REPRESENTATION_RELATIONSHIP_WITH_TRANSFORMATION(#17)
SHAPE_REPRESENTATION_RELATIONSHIP()
);
#72=(
REPRESENTATION_RELATIONSHIP($,$,#10676,#10673)
REPRESENTATION_RELATIONSHIP_WITH_TRANSFORMATION(#18)
SHAPE_REPRESENTATION_RELATIONSHIP()
);
#73=(
REPRESENTATION_RELATIONSHIP($,$,#10677,#10673)
REPRESENTATION_RELATIONSHIP_WITH_TRANSFORMATION(#19)
SHAPE_REPRESENTATION_RELATIONSHIP()
);
#74=(
REPRESENTATION_RELATIONSHIP($,$,#10678,#10673)
REPRESENTATION_RELATIONSHIP_WITH_TRANSFORMATION(#20)
SHAPE_REPRESENTATION_RELATIONSHIP()
);
#75=(
REPRESENTATION_RELATIONSHIP($,$,#10647,#10646)
REPRESENTATION_RELATIONSHIP_WITH_TRANSFORMATION(#21)
SHAPE_REPRESENTATION_RELATIONSHIP()
);
#76=(
REPRESENTATION_RELATIONSHIP($,$,#10648,#10646)
REPRESENTATION_RELATIONSHIP_WITH_TRANSFORMATION(#22)
SHAPE_REPRESENTATION_RELATIONSHIP()
);
#77=(
REPRESENTATION_RELATIONSHIP($,$,#10649,#10646)
REPRESENTATION_RELATIONSHIP_WITH_TRANSFORMATION(#23)
SHAPE_REPRESENTATION_RELATIONSHIP()
);
#78=(
REPRESENTATION_RELATIONSHIP($,$,#10650,#10646)
REPRESENTATION_RELATIONSHIP_WITH_TRANSFORMATION(#24)
SHAPE_REPRESENTATION_RELATIONSHIP()
);
#79=(
REPRESENTATION_RELATIONSHIP($,$,#10651,#10646)
REPRESENTATION_RELATIONSHIP_WITH_TRANSFORMATION(#25)
SHAPE_REPRESENTATION_RELATIONSHIP()
);
#80=(
REPRESENTATION_RELATIONSHIP($,$,#10652,#10646)
REPRESENTATION_RELATIONSHIP_WITH_TRANSFORMATION(#26)
SHAPE_REPRESENTATION_RELATIONSHIP()
);
#81=(
REPRESENTATION_RELATIONSHIP($,$,#10653,#10646)
REPRESENTATION_RELATIONSHIP_WITH_TRANSFORMATION(#27)
SHAPE_REPRESENTATION_RELATIONSHIP()
);
#82=(
REPRESENTATION_RELATIONSHIP($,$,#10654,#10646)
REPRESENTATION_RELATIONSHIP_WITH_TRANSFORMATION(#28)
SHAPE_REPRESENTATION_RELATIONSHIP()
);
#83=(
REPRESENTATION_RELATIONSHIP($,$,#10655,#10646)
REPRESENTATION_RELATIONSHIP_WITH_TRANSFORMATION(#29)
SHAPE_REPRESENTATION_RELATIONSHIP()
);
#84=(
REPRESENTATION_RELATIONSHIP($,$,#10654,#10646)
REPRESENTATION_RELATIONSHIP_WITH_TRANSFORMATION(#30)
SHAPE_REPRESENTATION_RELATIONSHIP()
);
#85=(
REPRESENTATION_RELATIONSHIP($,$,#10655,#10646)
REPRESENTATION_RELATIONSHIP_WITH_TRANSFORMATION(#31)
SHAPE_REPRESENTATION_RELATIONSHIP()
);
#86=(
REPRESENTATION_RELATIONSHIP($,$,#10654,#10646)
REPRESENTATION_RELATIONSHIP_WITH_TRANSFORMATION(#32)
SHAPE_REPRESENTATION_RELATIONSHIP()
);
#87=(
REPRESENTATION_RELATIONSHIP($,$,#10655,#10646)
REPRESENTATION_RELATIONSHIP_WITH_TRANSFORMATION(#33)
SHAPE_REPRESENTATION_RELATIONSHIP()
);
#88=(
REPRESENTATION_RELATIONSHIP($,$,#10654,#10646)
REPRESENTATION_RELATIONSHIP_WITH_TRANSFORMATION(#34)
SHAPE_REPRESENTATION_RELATIONSHIP()
);
#89=(
REPRESENTATION_RELATIONSHIP($,$,#10655,#10646)
REPRESENTATION_RELATIONSHIP_WITH_TRANSFORMATION(#35)
SHAPE_REPRESENTATION_RELATIONSHIP()
);
#90=(
REPRESENTATION_RELATIONSHIP($,$,#10656,#10646)
REPRESENTATION_RELATIONSHIP_WITH_TRANSFORMATION(#36)
SHAPE_REPRESENTATION_RELATIONSHIP()
);
#91=(
REPRESENTATION_RELATIONSHIP($,$,#10656,#10646)
REPRESENTATION_RELATIONSHIP_WITH_TRANSFORMATION(#37)
SHAPE_REPRESENTATION_RELATIONSHIP()
);
#92=(
REPRESENTATION_RELATIONSHIP($,$,#10679,#10646)
REPRESENTATION_RELATIONSHIP_WITH_TRANSFORMATION(#38)
SHAPE_REPRESENTATION_RELATIONSHIP()
);
#93=(
REPRESENTATION_RELATIONSHIP($,$,#10679,#10646)
REPRESENTATION_RELATIONSHIP_WITH_TRANSFORMATION(#39)
SHAPE_REPRESENTATION_RELATIONSHIP()
);
#94=(
REPRESENTATION_RELATIONSHIP($,$,#10679,#10646)
REPRESENTATION_RELATIONSHIP_WITH_TRANSFORMATION(#40)
SHAPE_REPRESENTATION_RELATIONSHIP()
);
#95=(
REPRESENTATION_RELATIONSHIP($,$,#10679,#10646)
REPRESENTATION_RELATIONSHIP_WITH_TRANSFORMATION(#41)
SHAPE_REPRESENTATION_RELATIONSHIP()
);
#96=(
REPRESENTATION_RELATIONSHIP($,$,#10679,#10646)
REPRESENTATION_RELATIONSHIP_WITH_TRANSFORMATION(#42)
SHAPE_REPRESENTATION_RELATIONSHIP()
);
#97=(
REPRESENTATION_RELATIONSHIP($,$,#10679,#10646)
REPRESENTATION_RELATIONSHIP_WITH_TRANSFORMATION(#43)
SHAPE_REPRESENTATION_RELATIONSHIP()
);
#98=(
REPRESENTATION_RELATIONSHIP($,$,#10679,#10646)
REPRESENTATION_RELATIONSHIP_WITH_TRANSFORMATION(#44)
SHAPE_REPRESENTATION_RELATIONSHIP()
);
#99=(
REPRESENTATION_RELATIONSHIP($,$,#10679,#10646)
REPRESENTATION_RELATIONSHIP_WITH_TRANSFORMATION(#45)
SHAPE_REPRESENTATION_RELATIONSHIP()
);
#100=(
REPRESENTATION_RELATIONSHIP($,$,#10663,#10662)
REPRESENTATION_RELATIONSHIP_WITH_TRANSFORMATION(#46)
SHAPE_REPRESENTATION_RELATIONSHIP()
);
#101=(
REPRESENTATION_RELATIONSHIP($,$,#10664,#10662)
REPRESENTATION_RELATIONSHIP_WITH_TRANSFORMATION(#47)
SHAPE_REPRESENTATION_RELATIONSHIP()
);
#102=(
REPRESENTATION_RELATIONSHIP($,$,#10665,#10662)
REPRESENTATION_RELATIONSHIP_WITH_TRANSFORMATION(#48)
SHAPE_REPRESENTATION_RELATIONSHIP()
);
#103=(
REPRESENTATION_RELATIONSHIP($,$,#10666,#10662)
REPRESENTATION_RELATIONSHIP_WITH_TRANSFORMATION(#49)
SHAPE_REPRESENTATION_RELATIONSHIP()
);
#104=(
REPRESENTATION_RELATIONSHIP($,$,#10667,#10662)
REPRESENTATION_RELATIONSHIP_WITH_TRANSFORMATION(#50)
SHAPE_REPRESENTATION_RELATIONSHIP()
);
#105=(
REPRESENTATION_RELATIONSHIP($,$,#10668,#10662)
REPRESENTATION_RELATIONSHIP_WITH_TRANSFORMATION(#51)
SHAPE_REPRESENTATION_RELATIONSHIP()
);
#106=(
REPRESENTATION_RELATIONSHIP($,$,#10669,#10662)
REPRESENTATION_RELATIONSHIP_WITH_TRANSFORMATION(#52)
SHAPE_REPRESENTATION_RELATIONSHIP()
);
#107=(
REPRESENTATION_RELATIONSHIP($,$,#10670,#10662)
REPRESENTATION_RELATIONSHIP_WITH_TRANSFORMATION(#53)
SHAPE_REPRESENTATION_RELATIONSHIP()
);
#108=(
REPRESENTATION_RELATIONSHIP($,$,#10671,#10662)
REPRESENTATION_RELATIONSHIP_WITH_TRANSFORMATION(#54)
SHAPE_REPRESENTATION_RELATIONSHIP()
);
#109=(
REPRESENTATION_RELATIONSHIP($,$,#10671,#10662)
REPRESENTATION_RELATIONSHIP_WITH_TRANSFORMATION(#55)
SHAPE_REPRESENTATION_RELATIONSHIP()
);
#110=(
REPRESENTATION_RELATIONSHIP($,$,#10672,#10662)
REPRESENTATION_RELATIONSHIP_WITH_TRANSFORMATION(#56)
SHAPE_REPRESENTATION_RELATIONSHIP()
);
#111=(
REPRESENTATION_RELATIONSHIP($,$,#10672,#10662)
REPRESENTATION_RELATIONSHIP_WITH_TRANSFORMATION(#57)
SHAPE_REPRESENTATION_RELATIONSHIP()
);
#112=(
REPRESENTATION_RELATIONSHIP($,$,#10673,#10662)
REPRESENTATION_RELATIONSHIP_WITH_TRANSFORMATION(#58)
SHAPE_REPRESENTATION_RELATIONSHIP()
);
#113=(
REPRESENTATION_RELATIONSHIP($,$,#10679,#10662)
REPRESENTATION_RELATIONSHIP_WITH_TRANSFORMATION(#59)
SHAPE_REPRESENTATION_RELATIONSHIP()
);
#114=(
REPRESENTATION_RELATIONSHIP($,$,#10681,#10680)
REPRESENTATION_RELATIONSHIP_WITH_TRANSFORMATION(#60)
SHAPE_REPRESENTATION_RELATIONSHIP()
);
#115=(
REPRESENTATION_RELATIONSHIP($,$,#10682,#10680)
REPRESENTATION_RELATIONSHIP_WITH_TRANSFORMATION(#61)
SHAPE_REPRESENTATION_RELATIONSHIP()
);
#116=(
REPRESENTATION_RELATIONSHIP($,$,#10646,#10645)
REPRESENTATION_RELATIONSHIP_WITH_TRANSFORMATION(#62)
SHAPE_REPRESENTATION_RELATIONSHIP()
);
#117=(
REPRESENTATION_RELATIONSHIP($,$,#10662,#10645)
REPRESENTATION_RELATIONSHIP_WITH_TRANSFORMATION(#63)
SHAPE_REPRESENTATION_RELATIONSHIP()
);
#118=(
REPRESENTATION_RELATIONSHIP($,$,#10680,#10645)
REPRESENTATION_RELATIONSHIP_WITH_TRANSFORMATION(#64)
SHAPE_REPRESENTATION_RELATIONSHIP()
);
#119=CONTEXT_DEPENDENT_SHAPE_REPRESENTATION(#65,#10570);
#120=CONTEXT_DEPENDENT_SHAPE_REPRESENTATION(#66,#10571);
#121=CONTEXT_DEPENDENT_SHAPE_REPRESENTATION(#67,#10572);
#122=CONTEXT_DEPENDENT_SHAPE_REPRESENTATION(#68,#10573);
#123=CONTEXT_DEPENDENT_SHAPE_REPRESENTATION(#69,#10574);
#124=CONTEXT_DEPENDENT_SHAPE_REPRESENTATION(#70,#10592);
#125=CONTEXT_DEPENDENT_SHAPE_REPRESENTATION(#71,#10593);
#126=CONTEXT_DEPENDENT_SHAPE_REPRESENTATION(#72,#10594);
#127=CONTEXT_DEPENDENT_SHAPE_REPRESENTATION(#73,#10595);
#128=CONTEXT_DEPENDENT_SHAPE_REPRESENTATION(#74,#10596);
#129=CONTEXT_DEPENDENT_SHAPE_REPRESENTATION(#75,#10598);
#130=CONTEXT_DEPENDENT_SHAPE_REPRESENTATION(#76,#10599);
#131=CONTEXT_DEPENDENT_SHAPE_REPRESENTATION(#77,#10600);
#132=CONTEXT_DEPENDENT_SHAPE_REPRESENTATION(#78,#10601);
#133=CONTEXT_DEPENDENT_SHAPE_REPRESENTATION(#79,#10602);
#134=CONTEXT_DEPENDENT_SHAPE_REPRESENTATION(#80,#10603);
#135=CONTEXT_DEPENDENT_SHAPE_REPRESENTATION(#81,#10604);
#136=CONTEXT_DEPENDENT_SHAPE_REPRESENTATION(#82,#10605);
#137=CONTEXT_DEPENDENT_SHAPE_REPRESENTATION(#83,#10606);
#138=CONTEXT_DEPENDENT_SHAPE_REPRESENTATION(#84,#10607);
#139=CONTEXT_DEPENDENT_SHAPE_REPRESENTATION(#85,#10608);
#140=CONTEXT_DEPENDENT_SHAPE_REPRESENTATION(#86,#10609);
#141=CONTEXT_DEPENDENT_SHAPE_REPRESENTATION(#87,#10610);
#142=CONTEXT_DEPENDENT_SHAPE_REPRESENTATION(#88,#10611);
#143=CONTEXT_DEPENDENT_SHAPE_REPRESENTATION(#89,#10612);
#144=CONTEXT_DEPENDENT_SHAPE_REPRESENTATION(#90,#10613);
#145=CONTEXT_DEPENDENT_SHAPE_REPRESENTATION(#91,#10614);
#146=CONTEXT_DEPENDENT_SHAPE_REPRESENTATION(#92,#10615);
#147=CONTEXT_DEPENDENT_SHAPE_REPRESENTATION(#93,#10616);
#148=CONTEXT_DEPENDENT_SHAPE_REPRESENTATION(#94,#10617);
#149=CONTEXT_DEPENDENT_SHAPE_REPRESENTATION(#95,#10618);
#150=CONTEXT_DEPENDENT_SHAPE_REPRESENTATION(#96,#10619);
#151=CONTEXT_DEPENDENT_SHAPE_REPRESENTATION(#97,#10620);
#152=CONTEXT_DEPENDENT_SHAPE_REPRESENTATION(#98,#10621);
#153=CONTEXT_DEPENDENT_SHAPE_REPRESENTATION(#99,#10622);
#154=CONTEXT_DEPENDENT_SHAPE_REPRESENTATION(#100,#10623);
#155=CONTEXT_DEPENDENT_SHAPE_REPRESENTATION(#101,#10624);
#156=CONTEXT_DEPENDENT_SHAPE_REPRESENTATION(#102,#10625);
#157=CONTEXT_DEPENDENT_SHAPE_REPRESENTATION(#103,#10626);
#158=CONTEXT_DEPENDENT_SHAPE_REPRESENTATION(#104,#10627);
#159=CONTEXT_DEPENDENT_SHAPE_REPRESENTATION(#105,#10628);
#160=CONTEXT_DEPENDENT_SHAPE_REPRESENTATION(#106,#10629);
#161=CONTEXT_DEPENDENT_SHAPE_REPRESENTATION(#107,#10630);
#162=CONTEXT_DEPENDENT_SHAPE_REPRESENTATION(#108,#10631);
#163=CONTEXT_DEPENDENT_SHAPE_REPRESENTATION(#109,#10632);
#164=CONTEXT_DEPENDENT_SHAPE_REPRESENTATION(#110,#10633);
#165=CONTEXT_DEPENDENT_SHAPE_REPRESENTATION(#111,#10634);
#166=CONTEXT_DEPENDENT_SHAPE_REPRESENTATION(#112,#10635);
#167=CONTEXT_DEPENDENT_SHAPE_REPRESENTATION(#113,#10636);
#168=CONTEXT_DEPENDENT_SHAPE_REPRESENTATION(#114,#10640);
#169=CONTEXT_DEPENDENT_SHAPE_REPRESENTATION(#115,#10641);
#170=CONTEXT_DEPENDENT_SHAPE_REPRESENTATION(#116,#10642);
#171=CONTEXT_DEPENDENT_SHAPE_REPRESENTATION(#117,#10643);
#172=CONTEXT_DEPENDENT_SHAPE_REPRESENTATION(#118,#10644);
#173=NEXT_ASSEMBLY_USAGE_OCCURRENCE('Inner ring:1','Inner ring:1',
'Inner ring:1',#10695,#10696,'Inner ring:1');
#174=NEXT_ASSEMBLY_USAGE_OCCURRENCE('Outer ring:1','Outer ring:1',
'Outer ring:1',#10695,#10697,'Outer ring:1');
#175=NEXT_ASSEMBLY_USAGE_OCCURRENCE('Balls:1','Balls:1','Balls:1',#10695,
#10698,'Balls:1');
#176=NEXT_ASSEMBLY_USAGE_OCCURRENCE('Cage:1','Cage:1','Cage:1',#10695,#10699,
'Cage:1');
#177=NEXT_ASSEMBLY_USAGE_OCCURRENCE('Seals 2RS:1','Seals 2RS:1',
'Seals 2RS:1',#10695,#10700,'Seals 2RS:1');
#178=NEXT_ASSEMBLY_USAGE_OCCURRENCE('Inner ring (1):1',
'Inner ring (1):1','Inner ring (1):1',#10712,#10713,'Inner ring (1):1');
#179=NEXT_ASSEMBLY_USAGE_OCCURRENCE('Outer ring (1):1',
'Outer ring (1):1','Outer ring (1):1',#10712,#10714,'Outer ring (1):1');
#180=NEXT_ASSEMBLY_USAGE_OCCURRENCE('Balls (1):1','Balls (1):1',
'Balls (1):1',#10712,#10715,'Balls (1):1');
#181=NEXT_ASSEMBLY_USAGE_OCCURRENCE('Cage (1):1','Cage (1):1',
'Cage (1):1',#10712,#10716,'Cage (1):1');
#182=NEXT_ASSEMBLY_USAGE_OCCURRENCE('Seals 2RS (1):1','Seals 2RS (1):1',
'Seals 2RS (1):1',#10712,#10717,'Seals 2RS (1):1');
#183=NEXT_ASSEMBLY_USAGE_OCCURRENCE('Base:1','Base:1','Base:1',#10685,#10686,
'Base:1');
#184=NEXT_ASSEMBLY_USAGE_OCCURRENCE('Bonded pad:1','Bonded pad:1',
'Bonded pad:1',#10685,#10687,'Bonded pad:1');
#185=NEXT_ASSEMBLY_USAGE_OCCURRENCE('Bonded pad (1):1',
'Bonded pad (1):1','Bonded pad (1):1',#10685,#10688,'Bonded pad (1):1');
#186=NEXT_ASSEMBLY_USAGE_OCCURRENCE('Bearing pedestal:1',
'Bearing pedestal:1','Bearing pedestal:1',#10685,#10689,
'Bearing pedestal:1');
#187=NEXT_ASSEMBLY_USAGE_OCCURRENCE('Outer race spacer:1',
'Outer race spacer:1','Outer race spacer:1',#10685,#10690,
'Outer race spacer:1');
#188=NEXT_ASSEMBLY_USAGE_OCCURRENCE('Bearing cap:1','Bearing cap:1',
'Bearing cap:1',#10685,#10691,'Bearing cap:1');
#189=NEXT_ASSEMBLY_USAGE_OCCURRENCE('Bearing cap (1):1',
'Bearing cap (1):1','Bearing cap (1):1',#10685,#10692,
'Bearing cap (1):1');
#190=NEXT_ASSEMBLY_USAGE_OCCURRENCE('Flat Washer - M6:2',
'Flat Washer - M6:2','Flat Washer - M6:2',#10685,#10693,
'Flat Washer - M6:2');
#191=NEXT_ASSEMBLY_USAGE_OCCURRENCE('M6x18 mounting screw:2',
'M6x18 mounting screw:2','M6x18 mounting screw:2',#10685,#10694,
'M6x18 mounting screw:2');
#192=NEXT_ASSEMBLY_USAGE_OCCURRENCE('Flat Washer - M6:3',
'Flat Washer - M6:3','Flat Washer - M6:3',#10685,#10693,
'Flat Washer - M6:3');
#193=NEXT_ASSEMBLY_USAGE_OCCURRENCE('M6x18 mounting screw:3',
'M6x18 mounting screw:3','M6x18 mounting screw:3',#10685,#10694,
'M6x18 mounting screw:3');
#194=NEXT_ASSEMBLY_USAGE_OCCURRENCE('Flat Washer - M6:4',
'Flat Washer - M6:4','Flat Washer - M6:4',#10685,#10693,
'Flat Washer - M6:4');
#195=NEXT_ASSEMBLY_USAGE_OCCURRENCE('M6x18 mounting screw:4',
'M6x18 mounting screw:4','M6x18 mounting screw:4',#10685,#10694,
'M6x18 mounting screw:4');
#196=NEXT_ASSEMBLY_USAGE_OCCURRENCE('Flat Washer - M6:5',
'Flat Washer - M6:5','Flat Washer - M6:5',#10685,#10693,
'Flat Washer - M6:5');
#197=NEXT_ASSEMBLY_USAGE_OCCURRENCE('M6x18 mounting screw:5',
'M6x18 mounting screw:5','M6x18 mounting screw:5',#10685,#10694,
'M6x18 mounting screw:5');
#198=NEXT_ASSEMBLY_USAGE_OCCURRENCE(
'Sealed Ball Bearing - 12 x 32 x 10 mm:2',
'Sealed Ball Bearing - 12 x 32 x 10 mm:2',
'Sealed Ball Bearing - 12 x 32 x 10 mm:2',#10685,#10695,
'Sealed Ball Bearing - 12 x 32 x 10 mm:2');
#199=NEXT_ASSEMBLY_USAGE_OCCURRENCE(
'Sealed Ball Bearing - 12 x 32 x 10 mm:3',
'Sealed Ball Bearing - 12 x 32 x 10 mm:3',
'Sealed Ball Bearing - 12 x 32 x 10 mm:3',#10685,#10695,
'Sealed Ball Bearing - 12 x 32 x 10 mm:3');
#200=NEXT_ASSEMBLY_USAGE_OCCURRENCE('Cap Screw - M4x16:2',
'Cap Screw - M4x16:2','Cap Screw - M4x16:2',#10685,#10718,
'Cap Screw - M4x16:2');
#201=NEXT_ASSEMBLY_USAGE_OCCURRENCE('Cap Screw - M4x16:3',
'Cap Screw - M4x16:3','Cap Screw - M4x16:3',#10685,#10718,
'Cap Screw - M4x16:3');
#202=NEXT_ASSEMBLY_USAGE_OCCURRENCE('Cap Screw - M4x16:4',
'Cap Screw - M4x16:4','Cap Screw - M4x16:4',#10685,#10718,
'Cap Screw - M4x16:4');
#203=NEXT_ASSEMBLY_USAGE_OCCURRENCE('Cap Screw - M4x16:5',
'Cap Screw - M4x16:5','Cap Screw - M4x16:5',#10685,#10718,
'Cap Screw - M4x16:5');
#204=NEXT_ASSEMBLY_USAGE_OCCURRENCE('Cap Screw - M4x16:6',
'Cap Screw - M4x16:6','Cap Screw - M4x16:6',#10685,#10718,
'Cap Screw - M4x16:6');
#205=NEXT_ASSEMBLY_USAGE_OCCURRENCE('Cap Screw - M4x16:7',
'Cap Screw - M4x16:7','Cap Screw - M4x16:7',#10685,#10718,
'Cap Screw - M4x16:7');
#206=NEXT_ASSEMBLY_USAGE_OCCURRENCE('Cap Screw - M4x16:8',
'Cap Screw - M4x16:8','Cap Screw - M4x16:8',#10685,#10718,
'Cap Screw - M4x16:8');
#207=NEXT_ASSEMBLY_USAGE_OCCURRENCE('Cap Screw - M4x16:9',
'Cap Screw - M4x16:9','Cap Screw - M4x16:9',#10685,#10718,
'Cap Screw - M4x16:9');
#208=NEXT_ASSEMBLY_USAGE_OCCURRENCE('Shaft:1','Shaft:1','Shaft:1',#10701,
#10702,'Shaft:1');
#209=NEXT_ASSEMBLY_USAGE_OCCURRENCE('Hand wheel:1','Hand wheel:1',
'Hand wheel:1',#10701,#10703,'Hand wheel:1');
#210=NEXT_ASSEMBLY_USAGE_OCCURRENCE('Inner race spacer:1',
'Inner race spacer:1','Inner race spacer:1',#10701,#10704,
'Inner race spacer:1');
#211=NEXT_ASSEMBLY_USAGE_OCCURRENCE('Shaft collar:1','Shaft collar:1',
'Shaft collar:1',#10701,#10705,'Shaft collar:1');
#212=NEXT_ASSEMBLY_USAGE_OCCURRENCE('Handle axle:1','Handle axle:1',
'Handle axle:1',#10701,#10706,'Handle axle:1');
#213=NEXT_ASSEMBLY_USAGE_OCCURRENCE('Handle inner spacer:1',
'Handle inner spacer:1','Handle inner spacer:1',#10701,#10707,
'Handle inner spacer:1');
#214=NEXT_ASSEMBLY_USAGE_OCCURRENCE('Handle axle keeper:1',
'Handle axle keeper:1','Handle axle keeper:1',#10701,#10708,
'Handle axle keeper:1');
#215=NEXT_ASSEMBLY_USAGE_OCCURRENCE('Parallel Key - 4x4x20:2',
'Parallel Key - 4x4x20:2','Parallel Key - 4x4x20:2',#10701,#10709,
'Parallel Key - 4x4x20:2');
#216=NEXT_ASSEMBLY_USAGE_OCCURRENCE('Socket Set Screw - M5x8:2',
'Socket Set Screw - M5x8:2','Socket Set Screw - M5x8:2',#10701,#10710,
'Socket Set Screw - M5x8:2');
#217=NEXT_ASSEMBLY_USAGE_OCCURRENCE('Socket Set Screw - M5x8:3',
'Socket Set Screw - M5x8:3','Socket Set Screw - M5x8:3',#10701,#10710,
'Socket Set Screw - M5x8:3');
#218=NEXT_ASSEMBLY_USAGE_OCCURRENCE('M4x10 handle screw:2',
'M4x10 handle screw:2','M4x10 handle screw:2',#10701,#10711,
'M4x10 handle screw:2');
#219=NEXT_ASSEMBLY_USAGE_OCCURRENCE('M4x10 handle screw:3',
'M4x10 handle screw:3','M4x10 handle screw:3',#10701,#10711,
'M4x10 handle screw:3');
#220=NEXT_ASSEMBLY_USAGE_OCCURRENCE(
'Sealed Ball Bearing - 10 x 30 x 9 mm:2',
'Sealed Ball Bearing - 10 x 30 x 9 mm:2',
'Sealed Ball Bearing - 10 x 30 x 9 mm:2',#10701,#10712,
'Sealed Ball Bearing - 10 x 30 x 9 mm:2');
#221=NEXT_ASSEMBLY_USAGE_OCCURRENCE('Cap Screw - M4x16:10',
'Cap Screw - M4x16:10','Cap Screw - M4x16:10',#10701,#10718,
'Cap Screw - M4x16:10');
#222=NEXT_ASSEMBLY_USAGE_OCCURRENCE('Revolving grip:1',
'Revolving grip:1','Revolving grip:1',#10719,#10720,'Revolving grip:1');
#223=NEXT_ASSEMBLY_USAGE_OCCURRENCE('Grip bearing cap:1',
'Grip bearing cap:1','Grip bearing cap:1',#10719,#10721,
'Grip bearing cap:1');
#224=NEXT_ASSEMBLY_USAGE_OCCURRENCE('Bearing stand:1','Bearing stand:1',
'Bearing stand:1',#10684,#10685,'Bearing stand:1');
#225=NEXT_ASSEMBLY_USAGE_OCCURRENCE('Wheel and shaft:1',
'Wheel and shaft:1','Wheel and shaft:1',#10684,#10701,
'Wheel and shaft:1');
#226=NEXT_ASSEMBLY_USAGE_OCCURRENCE('Revolving handle:1',
'Revolving handle:1','Revolving handle:1',#10684,#10719,
'Revolving handle:1');
#227=B_SPLINE_CURVE_WITH_KNOTS('',3,(#8677,#8678,#8679,#8680,#8681,#8682,
#8683,#8684,#8685,#8686,#8687,#8688,#8689,#8690,#8691,#8692,#8693,#8694,
#8695,#8696,#8697,#8698),.UNSPECIFIED.,.F.,.F.,(4,2,2,2,2,2,2,2,2,2,4),
(0.0591825211272536,0.157966726598481,0.236950089897721,0.315933453196962,
0.391576304923761,0.46721915665056,0.54286200837736,0.618504860104159,0.697488223403399,
0.77647158670264,0.875255792173867),.UNSPECIFIED.);
#228=B_SPLINE_CURVE_WITH_KNOTS('',3,(#8702,#8703,#8704,#8705,#8706,#8707,
#8708,#8709,#8710,#8711,#8712,#8713,#8714,#8715,#8716,#8717,#8718,#8719,
#8720,#8721,#8722,#8723),.UNSPECIFIED.,.F.,.F.,(4,2,2,2,2,2,2,2,2,2,4),
(0.0581119756758434,0.106553146291161,0.213106292582322,0.30849933801665,
0.386091982889075,0.4636846277615,0.541277272633925,0.61886991750635,0.714262962940678,
0.820816109231839,0.869257279847157),.UNSPECIFIED.);
#229=B_SPLINE_CURVE_WITH_KNOTS('',3,(#8729,#8730,#8731,#8732,#8733,#8734,
#8735,#8736,#8737,#8738,#8739,#8740,#8741,#8742,#8743,#8744,#8745,#8746,
#8747,#8748,#8749,#8750),.UNSPECIFIED.,.F.,.F.,(4,2,2,2,2,2,2,2,2,2,4),
(0.0581119756758434,0.106553146291161,0.213106292582322,0.30849933801665,
0.386091982889075,0.4636846277615,0.541277272633925,0.61886991750635,0.714262962940679,
0.820816109231839,0.869257279847157),.UNSPECIFIED.);
#230=B_SPLINE_CURVE_WITH_KNOTS('',3,(#8754,#8755,#8756,#8757,#8758,#8759,
#8760,#8761,#8762,#8763,#8764,#8765,#8766,#8767,#8768,#8769,#8770,#8771,
#8772,#8773,#8774,#8775),.UNSPECIFIED.,.F.,.F.,(4,2,2,2,2,2,2,2,2,2,4),
(0.0581119756758433,0.106553146291161,0.213106292582322,0.308499338016649,
0.386091982889075,0.4636846277615,0.541277272633925,0.61886991750635,0.714262962940678,
0.820816109231839,0.869257279847157),.UNSPECIFIED.);
#231=B_SPLINE_CURVE_WITH_KNOTS('',3,(#8784,#8785,#8786,#8787,#8788,#8789,
#8790,#8791,#8792,#8793,#8794,#8795,#8796,#8797,#8798,#8799,#8800,#8801,
#8802,#8803,#8804,#8805),.UNSPECIFIED.,.F.,.F.,(4,2,2,2,2,2,2,2,2,2,4),
(0.0581119756758433,0.106553146291161,0.213106292582322,0.30849933801665,
0.386091982889075,0.4636846277615,0.541277272633925,0.61886991750635,0.714262962940678,
0.820816109231839,0.869257279847157),.UNSPECIFIED.);
#232=B_SPLINE_CURVE_WITH_KNOTS('',3,(#8809,#8810,#8811,#8812,#8813,#8814,
#8815,#8816,#8817,#8818,#8819,#8820,#8821,#8822,#8823,#8824,#8825,#8826,
#8827,#8828,#8829,#8830),.UNSPECIFIED.,.F.,.F.,(4,2,2,2,2,2,2,2,2,2,4),
(0.0581119756758434,0.106553146291161,0.213106292582322,0.30849933801665,
0.386091982889075,0.4636846277615,0.541277272633925,0.61886991750635,0.714262962940678,
0.820816109231839,0.869257279847157),.UNSPECIFIED.);
#233=B_SPLINE_CURVE_WITH_KNOTS('',3,(#8834,#8835,#8836,#8837,#8838,#8839,
#8840,#8841,#8842,#8843,#8844,#8845,#8846,#8847,#8848,#8849,#8850,#8851,
#8852,#8853,#8854,#8855),.UNSPECIFIED.,.F.,.F.,(4,2,2,2,2,2,2,2,2,2,4),
(0.0581119756758434,0.106553146291161,0.213106292582322,0.30849933801665,
0.386091982889075,0.4636846277615,0.541277272633925,0.61886991750635,0.714262962940678,
0.820816109231839,0.869257279847157),.UNSPECIFIED.);
#234=B_SPLINE_CURVE_WITH_KNOTS('',3,(#8859,#8860,#8861,#8862,#8863,#8864,
#8865,#8866,#8867,#8868,#8869,#8870,#8871,#8872,#8873,#8874,#8875,#8876,
#8877,#8878,#8879,#8880),.UNSPECIFIED.,.F.,.F.,(4,2,2,2,2,2,2,2,2,2,4),
(0.0581119756758433,0.106553146291161,0.213106292582322,0.30849933801665,
0.386091982889075,0.4636846277615,0.541277272633925,0.61886991750635,0.714262962940678,
0.820816109231839,0.869257279847157),.UNSPECIFIED.);
#235=B_SPLINE_CURVE_WITH_KNOTS('',3,(#8888,#8889,#8890,#8891,#8892,#8893,
#8894,#8895,#8896,#8897,#8898,#8899,#8900,#8901,#8902,#8903,#8904,#8905,
#8906,#8907,#8908,#8909),.UNSPECIFIED.,.F.,.F.,(4,2,2,2,2,2,2,2,2,2,4),
(0.0591825211272536,0.157966726598481,0.236950089897721,0.315933453196962,
0.391576304923761,0.467219156650561,0.54286200837736,0.618504860104159,
0.697488223403399,0.77647158670264,0.875255792173867),.UNSPECIFIED.);
#236=B_SPLINE_CURVE_WITH_KNOTS('',3,(#8917,#8918,#8919,#8920,#8921,#8922,
#8923,#8924,#8925,#8926,#8927,#8928,#8929,#8930,#8931,#8932,#8933,#8934,
#8935,#8936,#8937,#8938),.UNSPECIFIED.,.F.,.F.,(4,2,2,2,2,2,2,2,2,2,4),
(0.0591825211272536,0.157966726598481,0.236950089897722,0.315933453196962,
0.391576304923761,0.467219156650561,0.54286200837736,0.618504860104159,
0.697488223403399,0.77647158670264,0.875255792173867),.UNSPECIFIED.);
#237=B_SPLINE_CURVE_WITH_KNOTS('',3,(#8948,#8949,#8950,#8951,#8952,#8953,
#8954,#8955,#8956,#8957,#8958,#8959,#8960,#8961,#8962,#8963,#8964,#8965,
#8966,#8967,#8968,#8969),.UNSPECIFIED.,.F.,.F.,(4,2,2,2,2,2,2,2,2,2,4),
(0.0591825211272536,0.157966726598481,0.236950089897721,0.315933453196962,
0.391576304923761,0.46721915665056,0.54286200837736,0.618504860104159,0.697488223403399,
0.77647158670264,0.875255792173867),.UNSPECIFIED.);
#238=B_SPLINE_CURVE_WITH_KNOTS('',3,(#8977,#8978,#8979,#8980,#8981,#8982,
#8983,#8984,#8985,#8986,#8987,#8988,#8989,#8990,#8991,#8992,#8993,#8994,
#8995,#8996,#8997,#8998),.UNSPECIFIED.,.F.,.F.,(4,2,2,2,2,2,2,2,2,2,4),
(0.0591825211272536,0.157966726598481,0.236950089897721,0.315933453196962,
0.391576304923761,0.46721915665056,0.542862008377359,0.618504860104159,
0.697488223403399,0.776471586702639,0.875255792173867),.UNSPECIFIED.);
#239=B_SPLINE_CURVE_WITH_KNOTS('',3,(#9006,#9007,#9008,#9009,#9010,#9011,
#9012,#9013,#9014,#9015,#9016,#9017,#9018,#9019,#9020,#9021,#9022,#9023,
#9024,#9025,#9026,#9027),.UNSPECIFIED.,.F.,.F.,(4,2,2,2,2,2,2,2,2,2,4),
(0.0591825211272536,0.157966726598481,0.236950089897721,0.315933453196962,
0.391576304923761,0.46721915665056,0.54286200837736,0.618504860104159,0.697488223403399,
0.77647158670264,0.875255792173867),.UNSPECIFIED.);
#240=B_SPLINE_CURVE_WITH_KNOTS('',3,(#9036,#9037,#9038,#9039,#9040,#9041,
#9042,#9043,#9044,#9045,#9046,#9047,#9048,#9049,#9050,#9051,#9052,#9053,
#9054,#9055,#9056,#9057),.UNSPECIFIED.,.F.,.F.,(4,2,2,2,2,2,2,2,2,2,4),
(0.0591825211272536,0.157966726598481,0.236950089897721,0.315933453196962,
0.391576304923761,0.46721915665056,0.542862008377359,0.618504860104159,
0.697488223403399,0.776471586702639,0.875255792173867),.UNSPECIFIED.);
#241=B_SPLINE_CURVE_WITH_KNOTS('',3,(#9168,#9169,#9170,#9171,#9172,#9173,
#9174,#9175,#9176,#9177),.UNSPECIFIED.,.F.,.F.,(4,2,2,2,4),(0.84783144568341,
0.878274576930948,0.958092875386314,1.03791117384168,1.06835430508922),
 .UNSPECIFIED.);
#242=B_SPLINE_CURVE_WITH_KNOTS('',3,(#9183,#9184,#9185,#9186,#9187,#9188,
#9189,#9190,#9191,#9192,#9193,#9194,#9195,#9196,#9197,#9198,#9199,#9200),
 .UNSPECIFIED.,.F.,.F.,(4,2,2,2,2,2,2,2,4),(0.,0.079216580773363,0.158433161546726,
0.23764869707457,0.316864232602414,0.396079768130259,0.475295303658103,
0.554511884431466,0.633728465204829),.UNSPECIFIED.);
#243=B_SPLINE_CURVE_WITH_KNOTS('',3,(#9201,#9202,#9203,#9204,#9205,#9206,
#9207,#9208,#9209,#9210,#9211,#9212,#9213,#9214,#9215,#9216,#9217,#9218),
 .UNSPECIFIED.,.F.,.F.,(4,2,2,2,2,2,2,2,4),(0.633728465204829,0.712945045978192,
0.792161626751555,0.871377162279399,0.950592697807243,1.02980823333509,
1.10902376886293,1.18824034963629,1.26745693040966),.UNSPECIFIED.);
#244=B_SPLINE_CURVE_WITH_KNOTS('',3,(#9221,#9222,#9223,#9224,#9225,#9226,
#9227,#9228,#9229,#9230),.UNSPECIFIED.,.F.,.F.,(4,2,2,2,4),(0.209102862092535,
0.239545993340072,0.319364291795438,0.399182590250804,0.429625721498342),
 .UNSPECIFIED.);
#245=B_SPLINE_CURVE_WITH_KNOTS('',3,(#9365,#9366,#9367,#9368,#9369,#9370,
#9371,#9372,#9373,#9374),.UNSPECIFIED.,.F.,.F.,(4,2,2,2,4),(0.818088904349178,
0.878131747417165,0.957937926194036,1.03774410497091,1.09778694803889),
 .UNSPECIFIED.);
#246=B_SPLINE_CURVE_WITH_KNOTS('',3,(#9380,#9381,#9382,#9383,#9384,#9385,
#9386,#9387,#9388,#9389,#9390,#9391,#9392,#9393,#9394,#9395,#9396,#9397),
 .UNSPECIFIED.,.F.,.F.,(4,2,2,2,2,2,2,2,4),(0.,0.0793157643915218,0.158631528783044,
0.237943615933649,0.317255703084255,0.396567790234861,0.475879877385467,
0.555195641776989,0.634511406168511),.UNSPECIFIED.);
#247=B_SPLINE_CURVE_WITH_KNOTS('',3,(#9398,#9399,#9400,#9401,#9402,#9403,
#9404,#9405,#9406,#9407,#9408,#9409,#9410,#9411,#9412,#9413,#9414,#9415),
 .UNSPECIFIED.,.F.,.F.,(4,2,2,2,2,2,2,2,4),(0.634511406168511,0.713827170560032,
0.793142934951554,0.87245502210216,0.951767109252766,1.03107919640337,1.11039128355398,
1.1897070479455,1.26902281233702),.UNSPECIFIED.);
#248=B_SPLINE_CURVE_WITH_KNOTS('',3,(#9418,#9419,#9420,#9421,#9422,#9423,
#9424,#9425,#9426,#9427),.UNSPECIFIED.,.F.,.F.,(4,2,2,2,4),(0.17946362021982,
0.239506463287808,0.319312642064679,0.39911882084155,0.459161663909536),
 .UNSPECIFIED.);
#249=B_SPLINE_CURVE_WITH_KNOTS('',3,(#9803,#9804,#9805,#9806,#9807,#9808,
#9809,#9810,#9811,#9812,#9813,#9814,#9815,#9816,#9817,#9818,#9819,#9820,
#9821,#9822,#9823,#9824),.UNSPECIFIED.,.F.,.F.,(4,2,2,2,2,2,2,2,2,2,4),
(0.0473477652366656,0.126350602536658,0.189525903804987,0.252701205073317,
0.313298422430275,0.373895639787233,0.434492857144191,0.495090074501149,
0.558265375769478,0.621440677037807,0.7004435143378),.UNSPECIFIED.);
#250=B_SPLINE_CURVE_WITH_KNOTS('',3,(#9828,#9829,#9830,#9831,#9832,#9833,
#9834,#9835,#9836,#9837,#9838,#9839,#9840,#9841,#9842,#9843,#9844,#9845,
#9846,#9847,#9848,#9849),.UNSPECIFIED.,.F.,.F.,(4,2,2,2,2,2,2,2,2,2,4),
(0.0464897534940957,0.0852567806515119,0.170513561303024,0.246687263103517,
0.308657850341199,0.370628437578881,0.432599024816563,0.494569612054245,
0.570743313854739,0.656000094506251,0.694767121663666),.UNSPECIFIED.);
#251=B_SPLINE_CURVE_WITH_KNOTS('',3,(#9855,#9856,#9857,#9858,#9859,#9860,
#9861,#9862,#9863,#9864,#9865,#9866,#9867,#9868,#9869,#9870,#9871,#9872,
#9873,#9874,#9875,#9876),.UNSPECIFIED.,.F.,.F.,(4,2,2,2,2,2,2,2,2,2,4),
(0.0464897534940957,0.0852567806515118,0.170513561303024,0.246687263103517,
0.308657850341199,0.370628437578881,0.432599024816563,0.494569612054245,
0.570743313854738,0.65600009450625,0.694767121663666),.UNSPECIFIED.);
#252=B_SPLINE_CURVE_WITH_KNOTS('',3,(#9880,#9881,#9882,#9883,#9884,#9885,
#9886,#9887,#9888,#9889,#9890,#9891,#9892,#9893,#9894,#9895,#9896,#9897,
#9898,#9899,#9900,#9901),.UNSPECIFIED.,.F.,.F.,(4,2,2,2,2,2,2,2,2,2,4),
(0.0464897534940957,0.0852567806515119,0.170513561303024,0.246687263103517,
0.308657850341199,0.370628437578881,0.432599024816563,0.494569612054245,
0.570743313854739,0.656000094506251,0.694767121663666),.UNSPECIFIED.);
#253=B_SPLINE_CURVE_WITH_KNOTS('',3,(#9905,#9906,#9907,#9908,#9909,#9910,
#9911,#9912,#9913,#9914,#9915,#9916),.UNSPECIFIED.,.F.,.F.,(4,2,2,2,2,4),
(0.0464897534940957,0.0852567806515119,0.170513561303024,0.246687263103517,
0.308657850341199,0.370628437578881),.UNSPECIFIED.);
#254=B_SPLINE_CURVE_WITH_KNOTS('',3,(#9921,#9922,#9923,#9924,#9925,#9926,
#9927,#9928,#9929,#9930,#9931,#9932),.UNSPECIFIED.,.F.,.F.,(4,2,2,2,2,4),
(0.370628437578881,0.432599024816563,0.494569612054245,0.570743313854738,
0.65600009450625,0.694767121663666),.UNSPECIFIED.);
#255=B_SPLINE_CURVE_WITH_KNOTS('',3,(#9936,#9937,#9938,#9939,#9940,#9941,
#9942,#9943,#9944,#9945,#9946,#9947,#9948,#9949,#9950,#9951,#9952,#9953,
#9954,#9955,#9956,#9957),.UNSPECIFIED.,.F.,.F.,(4,2,2,2,2,2,2,2,2,2,4),
(0.0464897534940957,0.0852567806515121,0.170513561303024,0.246687263103518,
0.308657850341199,0.370628437578881,0.432599024816563,0.494569612054245,
0.570743313854738,0.65600009450625,0.694767121663666),.UNSPECIFIED.);
#256=B_SPLINE_CURVE_WITH_KNOTS('',3,(#9961,#9962,#9963,#9964,#9965,#9966,
#9967,#9968,#9969,#9970,#9971,#9972,#9973,#9974,#9975,#9976,#9977,#9978,
#9979,#9980,#9981,#9982),.UNSPECIFIED.,.F.,.F.,(4,2,2,2,2,2,2,2,2,2,4),
(0.0464897534940957,0.0852567806515119,0.170513561303024,0.246687263103517,
0.308657850341199,0.370628437578881,0.432599024816563,0.494569612054245,
0.570743313854738,0.65600009450625,0.694767121663667),.UNSPECIFIED.);
#257=B_SPLINE_CURVE_WITH_KNOTS('',3,(#9986,#9987,#9988,#9989,#9990,#9991,
#9992,#9993,#9994,#9995,#9996,#9997,#9998,#9999,#10000,#10001,#10002,#10003,
#10004,#10005,#10006,#10007),.UNSPECIFIED.,.F.,.F.,(4,2,2,2,2,2,2,2,2,2,
4),(0.0464897534940957,0.0852567806515119,0.170513561303024,0.246687263103517,
0.308657850341199,0.370628437578881,0.432599024816563,0.494569612054245,
0.570743313854738,0.65600009450625,0.694767121663666),.UNSPECIFIED.);
#258=B_SPLINE_CURVE_WITH_KNOTS('',3,(#10011,#10012,#10013,#10014,#10015,
#10016,#10017,#10018,#10019,#10020,#10021,#10022,#10023,#10024,#10025,#10026,
#10027,#10028,#10029,#10030,#10031,#10032),.UNSPECIFIED.,.F.,.F.,(4,2,2,
2,2,2,2,2,2,2,4),(0.0464897534940957,0.0852567806515119,0.170513561303024,
0.246687263103517,0.308657850341199,0.370628437578881,0.432599024816563,
0.494569612054245,0.570743313854739,0.656000094506251,0.694767121663667),
 .UNSPECIFIED.);
#259=B_SPLINE_CURVE_WITH_KNOTS('',3,(#10040,#10041,#10042,#10043,#10044,
#10045,#10046,#10047,#10048,#10049,#10050,#10051,#10052,#10053,#10054,#10055,
#10056,#10057,#10058,#10059,#10060,#10061),.UNSPECIFIED.,.F.,.F.,(4,2,2,
2,2,2,2,2,2,2,4),(0.0473477652366656,0.126350602536658,0.189525903804987,
0.252701205073316,0.313298422430274,0.373895639787232,0.434492857144191,
0.495090074501149,0.558265375769478,0.621440677037807,0.7004435143378),
 .UNSPECIFIED.);
#260=B_SPLINE_CURVE_WITH_KNOTS('',3,(#10069,#10070,#10071,#10072,#10073,
#10074,#10075,#10076,#10077,#10078,#10079,#10080,#10081,#10082,#10083,#10084,
#10085,#10086,#10087,#10088,#10089,#10090),.UNSPECIFIED.,.F.,.F.,(4,2,2,
2,2,2,2,2,2,2,4),(0.0473477652366656,0.126350602536658,0.189525903804987,
0.252701205073317,0.313298422430275,0.373895639787233,0.434492857144191,
0.495090074501149,0.558265375769478,0.621440677037807,0.7004435143378),
 .UNSPECIFIED.);
#261=B_SPLINE_CURVE_WITH_KNOTS('',3,(#10099,#10100,#10101,#10102,#10103,
#10104,#10105,#10106,#10107,#10108,#10109,#10110),.UNSPECIFIED.,.F.,.F.,
(4,2,2,2,2,4),(0.0473477652366656,0.126350602536658,0.189525903804987,0.252701205073316,
0.313298422430275,0.373895639787233),.UNSPECIFIED.);
#262=B_SPLINE_CURVE_WITH_KNOTS('',3,(#10112,#10113,#10114,#10115,#10116,
#10117,#10118,#10119,#10120,#10121,#10122,#10123),.UNSPECIFIED.,.F.,.F.,
(4,2,2,2,2,4),(0.373895639787233,0.434492857144191,0.495090074501149,0.558265375769478,
0.621440677037807,0.7004435143378),.UNSPECIFIED.);
#263=B_SPLINE_CURVE_WITH_KNOTS('',3,(#10130,#10131,#10132,#10133,#10134,
#10135,#10136,#10137,#10138,#10139,#10140,#10141,#10142,#10143,#10144,#10145,
#10146,#10147,#10148,#10149,#10150,#10151),.UNSPECIFIED.,.F.,.F.,(4,2,2,
2,2,2,2,2,2,2,4),(0.0473477652366656,0.126350602536658,0.189525903804987,
0.252701205073316,0.313298422430275,0.373895639787233,0.434492857144191,
0.495090074501149,0.558265375769478,0.621440677037807,0.7004435143378),
 .UNSPECIFIED.);
#264=B_SPLINE_CURVE_WITH_KNOTS('',3,(#10159,#10160,#10161,#10162,#10163,
#10164,#10165,#10166,#10167,#10168,#10169,#10170,#10171,#10172,#10173,#10174,
#10175,#10176,#10177,#10178,#10179,#10180),.UNSPECIFIED.,.F.,.F.,(4,2,2,
2,2,2,2,2,2,2,4),(0.0473477652366656,0.126350602536658,0.189525903804987,
0.252701205073317,0.313298422430275,0.373895639787233,0.434492857144191,
0.495090074501149,0.558265375769478,0.621440677037807,0.7004435143378),
 .UNSPECIFIED.);
#265=B_SPLINE_CURVE_WITH_KNOTS('',3,(#10188,#10189,#10190,#10191,#10192,
#10193,#10194,#10195,#10196,#10197,#10198,#10199,#10200,#10201,#10202,#10203,
#10204,#10205,#10206,#10207,#10208,#10209),.UNSPECIFIED.,.F.,.F.,(4,2,2,
2,2,2,2,2,2,2,4),(0.0473477652366656,0.126350602536658,0.189525903804987,
0.252701205073316,0.313298422430275,0.373895639787233,0.434492857144191,
0.495090074501149,0.558265375769478,0.621440677037807,0.7004435143378),
 .UNSPECIFIED.);
#266=B_SPLINE_CURVE_WITH_KNOTS('',3,(#10218,#10219,#10220,#10221,#10222,
#10223,#10224,#10225,#10226,#10227,#10228,#10229,#10230,#10231,#10232,#10233,
#10234,#10235,#10236,#10237,#10238,#10239),.UNSPECIFIED.,.F.,.F.,(4,2,2,
2,2,2,2,2,2,2,4),(0.0473477652366656,0.126350602536658,0.189525903804987,
0.252701205073317,0.313298422430275,0.373895639787233,0.434492857144191,
0.495090074501149,0.558265375769478,0.621440677037807,0.7004435143378),
 .UNSPECIFIED.);
#267=SPHERICAL_SURFACE('',#5904,0.29765);
#268=SPHERICAL_SURFACE('',#5906,0.29765);
#269=SPHERICAL_SURFACE('',#5908,0.29765);
#270=SPHERICAL_SURFACE('',#5910,0.29765);
#271=SPHERICAL_SURFACE('',#5912,0.29765);
#272=SPHERICAL_SURFACE('',#5914,0.29765);
#273=SPHERICAL_SURFACE('',#5916,0.29765);
#274=SPHERICAL_SURFACE('',#5919,0.309556);
#275=SPHERICAL_SURFACE('',#5935,0.309556);
#276=SPHERICAL_SURFACE('',#5940,0.309556);
#277=SPHERICAL_SURFACE('',#5946,0.309556);
#278=SPHERICAL_SURFACE('',#5951,0.309556);
#279=SPHERICAL_SURFACE('',#5956,0.309556);
#280=SPHERICAL_SURFACE('',#5964,0.309556);
#281=SPHERICAL_SURFACE('',#6234,0.23815);
#282=SPHERICAL_SURFACE('',#6236,0.23815);
#283=SPHERICAL_SURFACE('',#6238,0.23815);
#284=SPHERICAL_SURFACE('',#6240,0.23815);
#285=SPHERICAL_SURFACE('',#6242,0.23815);
#286=SPHERICAL_SURFACE('',#6244,0.23815);
#287=SPHERICAL_SURFACE('',#6246,0.23815);
#288=SPHERICAL_SURFACE('',#6248,0.23815);
#289=SPHERICAL_SURFACE('',#6251,0.247676);
#290=SPHERICAL_SURFACE('',#6267,0.247676);
#291=SPHERICAL_SURFACE('',#6272,0.247676);
#292=SPHERICAL_SURFACE('',#6277,0.247676);
#293=SPHERICAL_SURFACE('',#6282,0.247676);
#294=SPHERICAL_SURFACE('',#6287,0.247676);
#295=SPHERICAL_SURFACE('',#6292,0.247676);
#296=SPHERICAL_SURFACE('',#6300,0.247676);
#297=TOROIDAL_SURFACE('',#5864,1.1,0.309556);
#298=TOROIDAL_SURFACE('',#5884,1.1,0.309556);
#299=TOROIDAL_SURFACE('',#6194,1.,0.247676);
#300=TOROIDAL_SURFACE('',#6214,1.,0.247676);
#301=CONICAL_SURFACE('',#5851,0.475,0.785398163397449);
#302=CONICAL_SURFACE('',#5855,0.485,0.785398163397448);
#303=CONICAL_SURFACE('',#5859,0.31,0.463647609000806);
#304=CONICAL_SURFACE('',#5875,0.63,0.785398163397448);
#305=CONICAL_SURFACE('',#5882,0.63,0.785398163397448);
#306=CONICAL_SURFACE('',#5895,1.57,0.785398163397449);
#307=CONICAL_SURFACE('',#5899,1.57,0.785398163397449);
#308=CONICAL_SURFACE('',#6130,0.18,0.785398163397448);
#309=CONICAL_SURFACE('',#6134,0.18,0.785398163397448);
#310=CONICAL_SURFACE('',#6142,0.18,0.785398163397449);
#311=CONICAL_SURFACE('',#6145,0.18,0.785398163397449);
#312=CONICAL_SURFACE('',#6161,0.235,0.785398163397448);
#313=CONICAL_SURFACE('',#6165,0.2125,0.785398163397448);
#314=CONICAL_SURFACE('',#6181,0.325,0.785398163397448);
#315=CONICAL_SURFACE('',#6185,0.335,0.785398163397448);
#316=CONICAL_SURFACE('',#6189,0.21,0.463647609000806);
#317=CONICAL_SURFACE('',#6205,0.53,0.785398163397448);
#318=CONICAL_SURFACE('',#6212,0.53,0.785398163397448);
#319=CONICAL_SURFACE('',#6225,1.47,0.785398163397449);
#320=CONICAL_SURFACE('',#6229,1.47,0.785398163397449);
#321=CONICAL_SURFACE('',#6329,0.325,0.785398163397448);
#322=CONICAL_SURFACE('',#6333,0.335,0.785398163397448);
#323=CONICAL_SURFACE('',#6337,0.21,0.463647609000806);
#324=CONICAL_SURFACE('',#6341,0.18,0.785398163397448);
#325=ORIENTED_CLOSED_SHELL('',*,#5302,.F.);
#326=ORIENTED_CLOSED_SHELL('',*,#5325,.F.);
#327=ORIENTED_CLOSED_SHELL('',*,#5341,.F.);
#328=BREP_WITH_VOIDS('Body1',#5303,(#325));
#329=BREP_WITH_VOIDS('Body1',#5326,(#326));
#330=BREP_WITH_VOIDS('Body1',#5340,(#327));
#331=SHAPE_REPRESENTATION_RELATIONSHIP('SRR','None',#10647,#363);
#332=SHAPE_REPRESENTATION_RELATIONSHIP('SRR','None',#10648,#364);
#333=SHAPE_REPRESENTATION_RELATIONSHIP('SRR','None',#10649,#365);
#334=SHAPE_REPRESENTATION_RELATIONSHIP('SRR','None',#10650,#366);
#335=SHAPE_REPRESENTATION_RELATIONSHIP('SRR','None',#10651,#367);
#336=SHAPE_REPRESENTATION_RELATIONSHIP('SRR','None',#10652,#368);
#337=SHAPE_REPRESENTATION_RELATIONSHIP('SRR','None',#10653,#369);
#338=SHAPE_REPRESENTATION_RELATIONSHIP('SRR','None',#10654,#370);
#339=SHAPE_REPRESENTATION_RELATIONSHIP('SRR','None',#10655,#371);
#340=SHAPE_REPRESENTATION_RELATIONSHIP('SRR','None',#10657,#372);
#341=SHAPE_REPRESENTATION_RELATIONSHIP('SRR','None',#10658,#373);
#342=SHAPE_REPRESENTATION_RELATIONSHIP('SRR','None',#10659,#374);
#343=SHAPE_REPRESENTATION_RELATIONSHIP('SRR','None',#10660,#375);
#344=SHAPE_REPRESENTATION_RELATIONSHIP('SRR','None',#10661,#376);
#345=SHAPE_REPRESENTATION_RELATIONSHIP('SRR','None',#10663,#377);
#346=SHAPE_REPRESENTATION_RELATIONSHIP('SRR','None',#10664,#378);
#347=SHAPE_REPRESENTATION_RELATIONSHIP('SRR','None',#10665,#379);
#348=SHAPE_REPRESENTATION_RELATIONSHIP('SRR','None',#10666,#380);
#349=SHAPE_REPRESENTATION_RELATIONSHIP('SRR','None',#10667,#381);
#350=SHAPE_REPRESENTATION_RELATIONSHIP('SRR','None',#10668,#382);
#351=SHAPE_REPRESENTATION_RELATIONSHIP('SRR','None',#10669,#383);
#352=SHAPE_REPRESENTATION_RELATIONSHIP('SRR','None',#10670,#384);
#353=SHAPE_REPRESENTATION_RELATIONSHIP('SRR','None',#10671,#385);
#354=SHAPE_REPRESENTATION_RELATIONSHIP('SRR','None',#10672,#386);
#355=SHAPE_REPRESENTATION_RELATIONSHIP('SRR','None',#10674,#387);
#356=SHAPE_REPRESENTATION_RELATIONSHIP('SRR','None',#10675,#388);
#357=SHAPE_REPRESENTATION_RELATIONSHIP('SRR','None',#10676,#389);
#358=SHAPE_REPRESENTATION_RELATIONSHIP('SRR','None',#10677,#390);
#359=SHAPE_REPRESENTATION_RELATIONSHIP('SRR','None',#10678,#391);
#360=SHAPE_REPRESENTATION_RELATIONSHIP('SRR','None',#10679,#392);
#361=SHAPE_REPRESENTATION_RELATIONSHIP('SRR','None',#10681,#393);
#362=SHAPE_REPRESENTATION_RELATIONSHIP('SRR','None',#10682,#394);
#363=ADVANCED_BREP_SHAPE_REPRESENTATION('',(#442),#10474);
#364=ADVANCED_BREP_SHAPE_REPRESENTATION('',(#443),#10475);
#365=ADVANCED_BREP_SHAPE_REPRESENTATION('',(#444),#10476);
#366=ADVANCED_BREP_SHAPE_REPRESENTATION('',(#445),#10477);
#367=ADVANCED_BREP_SHAPE_REPRESENTATION('',(#446),#10478);
#368=ADVANCED_BREP_SHAPE_REPRESENTATION('',(#447),#10479);
#369=ADVANCED_BREP_SHAPE_REPRESENTATION('',(#448),#10480);
#370=ADVANCED_BREP_SHAPE_REPRESENTATION('',(#449),#10481);
#371=ADVANCED_BREP_SHAPE_REPRESENTATION('',(#328),#10482);
#372=ADVANCED_BREP_SHAPE_REPRESENTATION('',(#450),#10484);
#373=ADVANCED_BREP_SHAPE_REPRESENTATION('',(#451),#10485);
#374=ADVANCED_BREP_SHAPE_REPRESENTATION('',(#452,#453,#454,#455,#456,#457,
#458),#10486);
#375=ADVANCED_BREP_SHAPE_REPRESENTATION('',(#459),#10487);
#376=ADVANCED_BREP_SHAPE_REPRESENTATION('',(#460,#461),#10488);
#377=ADVANCED_BREP_SHAPE_REPRESENTATION('',(#462),#10490);
#378=ADVANCED_BREP_SHAPE_REPRESENTATION('',(#463),#10491);
#379=ADVANCED_BREP_SHAPE_REPRESENTATION('',(#464),#10492);
#380=ADVANCED_BREP_SHAPE_REPRESENTATION('',(#465),#10493);
#381=ADVANCED_BREP_SHAPE_REPRESENTATION('',(#466),#10494);
#382=ADVANCED_BREP_SHAPE_REPRESENTATION('',(#467),#10495);
#383=ADVANCED_BREP_SHAPE_REPRESENTATION('',(#468),#10496);
#384=ADVANCED_BREP_SHAPE_REPRESENTATION('',(#469),#10497);
#385=ADVANCED_BREP_SHAPE_REPRESENTATION('',(#470),#10498);
#386=ADVANCED_BREP_SHAPE_REPRESENTATION('',(#329),#10499);
#387=ADVANCED_BREP_SHAPE_REPRESENTATION('',(#471),#10501);
#388=ADVANCED_BREP_SHAPE_REPRESENTATION('',(#472),#10502);
#389=ADVANCED_BREP_SHAPE_REPRESENTATION('',(#473,#474,#475,#476,#477,#478,
#479,#480),#10503);
#390=ADVANCED_BREP_SHAPE_REPRESENTATION('',(#481),#10504);
#391=ADVANCED_BREP_SHAPE_REPRESENTATION('',(#482,#483),#10505);
#392=ADVANCED_BREP_SHAPE_REPRESENTATION('',(#330),#10506);
#393=ADVANCED_BREP_SHAPE_REPRESENTATION('',(#484),#10508);
#394=ADVANCED_BREP_SHAPE_REPRESENTATION('',(#485),#10509);
#395=STYLED_ITEM('',(#10887),#442);
#396=STYLED_ITEM('',(#10922),#443);
#397=STYLED_ITEM('',(#10922),#444);
#398=STYLED_ITEM('',(#10908),#445);
#399=STYLED_ITEM('',(#10908),#446);
#400=STYLED_ITEM('',(#10908),#447);
#401=STYLED_ITEM('',(#10908),#448);
#402=STYLED_ITEM('',(#10915),#449);
#403=STYLED_ITEM('',(#10915),#328);
#404=STYLED_ITEM('',(#10908),#450);
#405=STYLED_ITEM('',(#10908),#451);
#406=STYLED_ITEM('',(#10908),#452);
#407=STYLED_ITEM('',(#10908),#453);
#408=STYLED_ITEM('',(#10908),#454);
#409=STYLED_ITEM('',(#10908),#455);
#410=STYLED_ITEM('',(#10908),#456);
#411=STYLED_ITEM('',(#10908),#457);
#412=STYLED_ITEM('',(#10908),#458);
#413=STYLED_ITEM('',(#10908),#459);
#414=STYLED_ITEM('',(#10908),#460);
#415=STYLED_ITEM('',(#10908),#461);
#416=STYLED_ITEM('',(#10908),#462);
#417=STYLED_ITEM('',(#10901),#463);
#418=STYLED_ITEM('',(#10908),#464);
#419=STYLED_ITEM('',(#10908),#465);
#420=STYLED_ITEM('',(#10908),#466);
#421=STYLED_ITEM('',(#10894),#467);
#422=STYLED_ITEM('',(#10908),#468);
#423=STYLED_ITEM('',(#10908),#469);
#424=STYLED_ITEM('',(#10915),#470);
#425=STYLED_ITEM('',(#10915),#329);
#426=STYLED_ITEM('',(#10908),#471);
#427=STYLED_ITEM('',(#10908),#472);
#428=STYLED_ITEM('',(#10908),#473);
#429=STYLED_ITEM('',(#10908),#474);
#430=STYLED_ITEM('',(#10908),#475);
#431=STYLED_ITEM('',(#10908),#476);
#432=STYLED_ITEM('',(#10908),#477);
#433=STYLED_ITEM('',(#10908),#478);
#434=STYLED_ITEM('',(#10908),#479);
#435=STYLED_ITEM('',(#10908),#480);
#436=STYLED_ITEM('',(#10908),#481);
#437=STYLED_ITEM('',(#10908),#482);
#438=STYLED_ITEM('',(#10908),#483);
#439=STYLED_ITEM('',(#10915),#330);
#440=STYLED_ITEM('',(#10915),#484);
#441=STYLED_ITEM('',(#10908),#485);
#442=MANIFOLD_SOLID_BREP('Body1',#5294);
#443=MANIFOLD_SOLID_BREP('Body1',#5295);
#444=MANIFOLD_SOLID_BREP('Body1',#5296);
#445=MANIFOLD_SOLID_BREP('Body1',#5297);
#446=MANIFOLD_SOLID_BREP('Body1',#5298);
#447=MANIFOLD_SOLID_BREP('Body1',#5299);
#448=MANIFOLD_SOLID_BREP('Body1',#5300);
#449=MANIFOLD_SOLID_BREP('Body1',#5301);
#450=MANIFOLD_SOLID_BREP('Body1',#5304);
#451=MANIFOLD_SOLID_BREP('Body1',#5305);
#452=MANIFOLD_SOLID_BREP('Body1',#5306);
#453=MANIFOLD_SOLID_BREP('Body2',#5307);
#454=MANIFOLD_SOLID_BREP('Body3',#5308);
#455=MANIFOLD_SOLID_BREP('Body4',#5309);
#456=MANIFOLD_SOLID_BREP('Body5',#5310);
#457=MANIFOLD_SOLID_BREP('Body6',#5311);
#458=MANIFOLD_SOLID_BREP('Body7',#5312);
#459=MANIFOLD_SOLID_BREP('Continuous crown cage',#5313);
#460=MANIFOLD_SOLID_BREP('Body1',#5314);
#461=MANIFOLD_SOLID_BREP('Body2',#5315);
#462=MANIFOLD_SOLID_BREP('Body1',#5316);
#463=MANIFOLD_SOLID_BREP('Body1',#5317);
#464=MANIFOLD_SOLID_BREP('Body1',#5318);
#465=MANIFOLD_SOLID_BREP('Body1',#5319);
#466=MANIFOLD_SOLID_BREP('Body1',#5320);
#467=MANIFOLD_SOLID_BREP('Body1',#5321);
#468=MANIFOLD_SOLID_BREP('Body1',#5322);
#469=MANIFOLD_SOLID_BREP('Body1',#5323);
#470=MANIFOLD_SOLID_BREP('Body1',#5324);
#471=MANIFOLD_SOLID_BREP('Body1',#5327);
#472=MANIFOLD_SOLID_BREP('Body1',#5328);
#473=MANIFOLD_SOLID_BREP('Body1',#5329);
#474=MANIFOLD_SOLID_BREP('Body2',#5330);
#475=MANIFOLD_SOLID_BREP('Body3',#5331);
#476=MANIFOLD_SOLID_BREP('Body4',#5332);
#477=MANIFOLD_SOLID_BREP('Body5',#5333);
#478=MANIFOLD_SOLID_BREP('Body6',#5334);
#479=MANIFOLD_SOLID_BREP('Body7',#5335);
#480=MANIFOLD_SOLID_BREP('Body8',#5336);
#481=MANIFOLD_SOLID_BREP('Continuous crown cage',#5337);
#482=MANIFOLD_SOLID_BREP('Body1',#5338);
#483=MANIFOLD_SOLID_BREP('Body2',#5339);
#484=MANIFOLD_SOLID_BREP('Body1',#5342);
#485=MANIFOLD_SOLID_BREP('Body1',#5343);
#486=FACE_BOUND('',#1091,.T.);
#487=FACE_BOUND('',#1092,.T.);
#488=FACE_BOUND('',#1093,.T.);
#489=FACE_BOUND('',#1094,.T.);
#490=FACE_BOUND('',#1096,.T.);
#491=FACE_BOUND('',#1097,.T.);
#492=FACE_BOUND('',#1098,.T.);
#493=FACE_BOUND('',#1099,.T.);
#494=FACE_BOUND('',#1122,.T.);
#495=FACE_BOUND('',#1123,.T.);
#496=FACE_BOUND('',#1125,.T.);
#497=FACE_BOUND('',#1126,.T.);
#498=FACE_BOUND('',#1130,.T.);
#499=FACE_BOUND('',#1131,.T.);
#500=FACE_BOUND('',#1132,.T.);
#501=FACE_BOUND('',#1133,.T.);
#502=FACE_BOUND('',#1134,.T.);
#503=FACE_BOUND('',#1137,.T.);
#504=FACE_BOUND('',#1138,.T.);
#505=FACE_BOUND('',#1139,.T.);
#506=FACE_BOUND('',#1140,.T.);
#507=FACE_BOUND('',#1141,.T.);
#508=FACE_BOUND('',#1145,.T.);
#509=FACE_BOUND('',#1146,.T.);
#510=FACE_BOUND('',#1147,.T.);
#511=FACE_BOUND('',#1148,.T.);
#512=FACE_BOUND('',#1152,.T.);
#513=FACE_BOUND('',#1154,.T.);
#514=FACE_BOUND('',#1161,.T.);
#515=FACE_BOUND('',#1165,.T.);
#516=FACE_BOUND('',#1166,.T.);
#517=FACE_BOUND('',#1167,.T.);
#518=FACE_BOUND('',#1168,.T.);
#519=FACE_BOUND('',#1169,.T.);
#520=FACE_BOUND('',#1171,.T.);
#521=FACE_BOUND('',#1172,.T.);
#522=FACE_BOUND('',#1173,.T.);
#523=FACE_BOUND('',#1174,.T.);
#524=FACE_BOUND('',#1175,.T.);
#525=FACE_BOUND('',#1182,.T.);
#526=FACE_BOUND('',#1186,.T.);
#527=FACE_BOUND('',#1187,.T.);
#528=FACE_BOUND('',#1188,.T.);
#529=FACE_BOUND('',#1189,.T.);
#530=FACE_BOUND('',#1190,.T.);
#531=FACE_BOUND('',#1192,.T.);
#532=FACE_BOUND('',#1193,.T.);
#533=FACE_BOUND('',#1194,.T.);
#534=FACE_BOUND('',#1195,.T.);
#535=FACE_BOUND('',#1196,.T.);
#536=FACE_BOUND('',#1200,.T.);
#537=FACE_BOUND('',#1202,.T.);
#538=FACE_BOUND('',#1217,.T.);
#539=FACE_BOUND('',#1225,.T.);
#540=FACE_BOUND('',#1228,.T.);
#541=FACE_BOUND('',#1233,.T.);
#542=FACE_BOUND('',#1238,.T.);
#543=FACE_BOUND('',#1263,.T.);
#544=FACE_BOUND('',#1266,.T.);
#545=FACE_BOUND('',#1269,.T.);
#546=FACE_BOUND('',#1272,.T.);
#547=FACE_BOUND('',#1275,.T.);
#548=FACE_BOUND('',#1283,.T.);
#549=FACE_BOUND('',#1285,.T.);
#550=FACE_BOUND('',#1288,.T.);
#551=FACE_BOUND('',#1301,.T.);
#552=FACE_BOUND('',#1303,.T.);
#553=FACE_BOUND('',#1307,.T.);
#554=FACE_BOUND('',#1308,.T.);
#555=FACE_BOUND('',#1309,.T.);
#556=FACE_BOUND('',#1317,.T.);
#557=FACE_BOUND('',#1318,.T.);
#558=FACE_BOUND('',#1319,.T.);
#559=FACE_BOUND('',#1323,.T.);
#560=FACE_BOUND('',#1324,.T.);
#561=FACE_BOUND('',#1325,.T.);
#562=FACE_BOUND('',#1326,.T.);
#563=FACE_BOUND('',#1328,.T.);
#564=FACE_BOUND('',#1332,.T.);
#565=FACE_BOUND('',#1334,.T.);
#566=FACE_BOUND('',#1339,.T.);
#567=FACE_BOUND('',#1341,.T.);
#568=FACE_BOUND('',#1343,.T.);
#569=FACE_BOUND('',#1345,.T.);
#570=FACE_BOUND('',#1351,.T.);
#571=FACE_BOUND('',#1352,.T.);
#572=FACE_BOUND('',#1353,.T.);
#573=FACE_BOUND('',#1356,.T.);
#574=FACE_BOUND('',#1360,.T.);
#575=FACE_BOUND('',#1361,.T.);
#576=FACE_BOUND('',#1363,.T.);
#577=FACE_BOUND('',#1367,.T.);
#578=FACE_BOUND('',#1369,.T.);
#579=FACE_BOUND('',#1373,.T.);
#580=FACE_BOUND('',#1375,.T.);
#581=FACE_BOUND('',#1398,.T.);
#582=FACE_BOUND('',#1417,.T.);
#583=FACE_BOUND('',#1425,.T.);
#584=FACE_BOUND('',#1428,.T.);
#585=FACE_BOUND('',#1433,.T.);
#586=FACE_BOUND('',#1438,.T.);
#587=FACE_BOUND('',#1466,.T.);
#588=FACE_BOUND('',#1469,.T.);
#589=FACE_BOUND('',#1472,.T.);
#590=FACE_BOUND('',#1475,.T.);
#591=FACE_BOUND('',#1478,.T.);
#592=FACE_BOUND('',#1485,.T.);
#593=FACE_BOUND('',#1500,.T.);
#594=FACE_BOUND('',#1504,.T.);
#595=FACE_BOUND('',#1506,.T.);
#596=FACE_BOUND('',#1510,.T.);
#597=FACE_BOUND('',#1512,.T.);
#598=PLANE('',#5712);
#599=PLANE('',#5713);
#600=PLANE('',#5714);
#601=PLANE('',#5715);
#602=PLANE('',#5716);
#603=PLANE('',#5717);
#604=PLANE('',#5719);
#605=PLANE('',#5720);
#606=PLANE('',#5721);
#607=PLANE('',#5722);
#608=PLANE('',#5723);
#609=PLANE('',#5724);
#610=PLANE('',#5726);
#611=PLANE('',#5727);
#612=PLANE('',#5728);
#613=PLANE('',#5729);
#614=PLANE('',#5730);
#615=PLANE('',#5731);
#616=PLANE('',#5760);
#617=PLANE('',#5761);
#618=PLANE('',#5762);
#619=PLANE('',#5763);
#620=PLANE('',#5764);
#621=PLANE('',#5765);
#622=PLANE('',#5766);
#623=PLANE('',#5767);
#624=PLANE('',#5768);
#625=PLANE('',#5769);
#626=PLANE('',#5777);
#627=PLANE('',#5778);
#628=PLANE('',#5795);
#629=PLANE('',#5802);
#630=PLANE('',#5803);
#631=PLANE('',#5820);
#632=PLANE('',#5827);
#633=PLANE('',#5828);
#634=PLANE('',#5836);
#635=PLANE('',#5837);
#636=PLANE('',#5839);
#637=PLANE('',#5840);
#638=PLANE('',#5841);
#639=PLANE('',#5842);
#640=PLANE('',#5843);
#641=PLANE('',#5844);
#642=PLANE('',#5845);
#643=PLANE('',#5846);
#644=PLANE('',#5847);
#645=PLANE('',#5849);
#646=PLANE('',#5857);
#647=PLANE('',#5877);
#648=PLANE('',#5880);
#649=PLANE('',#5892);
#650=PLANE('',#5901);
#651=PLANE('',#5932);
#652=PLANE('',#5937);
#653=PLANE('',#5942);
#654=PLANE('',#5948);
#655=PLANE('',#5953);
#656=PLANE('',#5962);
#657=PLANE('',#5966);
#658=PLANE('',#5967);
#659=PLANE('',#5969);
#660=PLANE('',#5974);
#661=PLANE('',#5977);
#662=PLANE('',#5982);
#663=PLANE('',#5992);
#664=PLANE('',#5993);
#665=PLANE('',#5995);
#666=PLANE('',#5996);
#667=PLANE('',#5997);
#668=PLANE('',#5999);
#669=PLANE('',#6002);
#670=PLANE('',#6010);
#671=PLANE('',#6011);
#672=PLANE('',#6019);
#673=PLANE('',#6024);
#674=PLANE('',#6025);
#675=PLANE('',#6026);
#676=PLANE('',#6027);
#677=PLANE('',#6028);
#678=PLANE('',#6033);
#679=PLANE('',#6034);
#680=PLANE('',#6035);
#681=PLANE('',#6045);
#682=PLANE('',#6046);
#683=PLANE('',#6049);
#684=PLANE('',#6050);
#685=PLANE('',#6051);
#686=PLANE('',#6061);
#687=PLANE('',#6069);
#688=PLANE('',#6070);
#689=PLANE('',#6072);
#690=PLANE('',#6077);
#691=PLANE('',#6084);
#692=PLANE('',#6085);
#693=PLANE('',#6090);
#694=PLANE('',#6097);
#695=PLANE('',#6102);
#696=PLANE('',#6108);
#697=PLANE('',#6109);
#698=PLANE('',#6117);
#699=PLANE('',#6118);
#700=PLANE('',#6126);
#701=PLANE('',#6127);
#702=PLANE('',#6129);
#703=PLANE('',#6133);
#704=PLANE('',#6139);
#705=PLANE('',#6140);
#706=PLANE('',#6141);
#707=PLANE('',#6144);
#708=PLANE('',#6149);
#709=PLANE('',#6150);
#710=PLANE('',#6152);
#711=PLANE('',#6153);
#712=PLANE('',#6154);
#713=PLANE('',#6155);
#714=PLANE('',#6156);
#715=PLANE('',#6157);
#716=PLANE('',#6158);
#717=PLANE('',#6159);
#718=PLANE('',#6167);
#719=PLANE('',#6169);
#720=PLANE('',#6170);
#721=PLANE('',#6171);
#722=PLANE('',#6172);
#723=PLANE('',#6173);
#724=PLANE('',#6174);
#725=PLANE('',#6175);
#726=PLANE('',#6176);
#727=PLANE('',#6177);
#728=PLANE('',#6179);
#729=PLANE('',#6187);
#730=PLANE('',#6207);
#731=PLANE('',#6210);
#732=PLANE('',#6222);
#733=PLANE('',#6231);
#734=PLANE('',#6264);
#735=PLANE('',#6269);
#736=PLANE('',#6274);
#737=PLANE('',#6279);
#738=PLANE('',#6284);
#739=PLANE('',#6289);
#740=PLANE('',#6298);
#741=PLANE('',#6302);
#742=PLANE('',#6303);
#743=PLANE('',#6305);
#744=PLANE('',#6310);
#745=PLANE('',#6313);
#746=PLANE('',#6318);
#747=PLANE('',#6327);
#748=PLANE('',#6335);
#749=PLANE('',#6343);
#750=PLANE('',#6344);
#751=PLANE('',#6345);
#752=PLANE('',#6346);
#753=PLANE('',#6347);
#754=PLANE('',#6348);
#755=PLANE('',#6349);
#756=PLANE('',#6350);
#757=PLANE('',#6351);
#758=PLANE('',#6396);
#759=PLANE('',#6403);
#760=PLANE('',#6404);
#761=PLANE('',#6412);
#762=PLANE('',#6413);
#763=FACE_OUTER_BOUND('',#1082,.T.);
#764=FACE_OUTER_BOUND('',#1083,.T.);
#765=FACE_OUTER_BOUND('',#1084,.T.);
#766=FACE_OUTER_BOUND('',#1085,.T.);
#767=FACE_OUTER_BOUND('',#1086,.T.);
#768=FACE_OUTER_BOUND('',#1087,.T.);
#769=FACE_OUTER_BOUND('',#1088,.T.);
#770=FACE_OUTER_BOUND('',#1089,.T.);
#771=FACE_OUTER_BOUND('',#1090,.T.);
#772=FACE_OUTER_BOUND('',#1095,.T.);
#773=FACE_OUTER_BOUND('',#1100,.T.);
#774=FACE_OUTER_BOUND('',#1101,.T.);
#775=FACE_OUTER_BOUND('',#1102,.T.);
#776=FACE_OUTER_BOUND('',#1103,.T.);
#777=FACE_OUTER_BOUND('',#1104,.T.);
#778=FACE_OUTER_BOUND('',#1105,.T.);
#779=FACE_OUTER_BOUND('',#1106,.T.);
#780=FACE_OUTER_BOUND('',#1107,.T.);
#781=FACE_OUTER_BOUND('',#1108,.T.);
#782=FACE_OUTER_BOUND('',#1109,.T.);
#783=FACE_OUTER_BOUND('',#1110,.T.);
#784=FACE_OUTER_BOUND('',#1111,.T.);
#785=FACE_OUTER_BOUND('',#1112,.T.);
#786=FACE_OUTER_BOUND('',#1113,.T.);
#787=FACE_OUTER_BOUND('',#1114,.T.);
#788=FACE_OUTER_BOUND('',#1115,.T.);
#789=FACE_OUTER_BOUND('',#1116,.T.);
#790=FACE_OUTER_BOUND('',#1117,.T.);
#791=FACE_OUTER_BOUND('',#1118,.T.);
#792=FACE_OUTER_BOUND('',#1119,.T.);
#793=FACE_OUTER_BOUND('',#1120,.T.);
#794=FACE_OUTER_BOUND('',#1121,.T.);
#795=FACE_OUTER_BOUND('',#1124,.T.);
#796=FACE_OUTER_BOUND('',#1127,.T.);
#797=FACE_OUTER_BOUND('',#1128,.T.);
#798=FACE_OUTER_BOUND('',#1129,.T.);
#799=FACE_OUTER_BOUND('',#1135,.T.);
#800=FACE_OUTER_BOUND('',#1136,.T.);
#801=FACE_OUTER_BOUND('',#1142,.T.);
#802=FACE_OUTER_BOUND('',#1143,.T.);
#803=FACE_OUTER_BOUND('',#1144,.T.);
#804=FACE_OUTER_BOUND('',#1149,.T.);
#805=FACE_OUTER_BOUND('',#1150,.T.);
#806=FACE_OUTER_BOUND('',#1151,.T.);
#807=FACE_OUTER_BOUND('',#1153,.T.);
#808=FACE_OUTER_BOUND('',#1155,.T.);
#809=FACE_OUTER_BOUND('',#1156,.T.);
#810=FACE_OUTER_BOUND('',#1157,.T.);
#811=FACE_OUTER_BOUND('',#1158,.T.);
#812=FACE_OUTER_BOUND('',#1159,.T.);
#813=FACE_OUTER_BOUND('',#1160,.T.);
#814=FACE_OUTER_BOUND('',#1162,.T.);
#815=FACE_OUTER_BOUND('',#1163,.T.);
#816=FACE_OUTER_BOUND('',#1164,.T.);
#817=FACE_OUTER_BOUND('',#1170,.T.);
#818=FACE_OUTER_BOUND('',#1176,.T.);
#819=FACE_OUTER_BOUND('',#1177,.T.);
#820=FACE_OUTER_BOUND('',#1178,.T.);
#821=FACE_OUTER_BOUND('',#1179,.T.);
#822=FACE_OUTER_BOUND('',#1180,.T.);
#823=FACE_OUTER_BOUND('',#1181,.T.);
#824=FACE_OUTER_BOUND('',#1183,.T.);
#825=FACE_OUTER_BOUND('',#1184,.T.);
#826=FACE_OUTER_BOUND('',#1185,.T.);
#827=FACE_OUTER_BOUND('',#1191,.T.);
#828=FACE_OUTER_BOUND('',#1197,.T.);
#829=FACE_OUTER_BOUND('',#1198,.T.);
#830=FACE_OUTER_BOUND('',#1199,.T.);
#831=FACE_OUTER_BOUND('',#1201,.T.);
#832=FACE_OUTER_BOUND('',#1203,.T.);
#833=FACE_OUTER_BOUND('',#1204,.T.);
#834=FACE_OUTER_BOUND('',#1205,.T.);
#835=FACE_OUTER_BOUND('',#1206,.T.);
#836=FACE_OUTER_BOUND('',#1207,.T.);
#837=FACE_OUTER_BOUND('',#1208,.T.);
#838=FACE_OUTER_BOUND('',#1209,.T.);
#839=FACE_OUTER_BOUND('',#1210,.T.);
#840=FACE_OUTER_BOUND('',#1211,.T.);
#841=FACE_OUTER_BOUND('',#1212,.T.);
#842=FACE_OUTER_BOUND('',#1213,.T.);
#843=FACE_OUTER_BOUND('',#1214,.T.);
#844=FACE_OUTER_BOUND('',#1215,.T.);
#845=FACE_OUTER_BOUND('',#1216,.T.);
#846=FACE_OUTER_BOUND('',#1218,.T.);
#847=FACE_OUTER_BOUND('',#1219,.T.);
#848=FACE_OUTER_BOUND('',#1220,.T.);
#849=FACE_OUTER_BOUND('',#1221,.T.);
#850=FACE_OUTER_BOUND('',#1222,.T.);
#851=FACE_OUTER_BOUND('',#1223,.T.);
#852=FACE_OUTER_BOUND('',#1224,.T.);
#853=FACE_OUTER_BOUND('',#1226,.T.);
#854=FACE_OUTER_BOUND('',#1227,.T.);
#855=FACE_OUTER_BOUND('',#1229,.T.);
#856=FACE_OUTER_BOUND('',#1230,.T.);
#857=FACE_OUTER_BOUND('',#1231,.T.);
#858=FACE_OUTER_BOUND('',#1232,.T.);
#859=FACE_OUTER_BOUND('',#1234,.T.);
#860=FACE_OUTER_BOUND('',#1235,.T.);
#861=FACE_OUTER_BOUND('',#1236,.T.);
#862=FACE_OUTER_BOUND('',#1237,.T.);
#863=FACE_OUTER_BOUND('',#1239,.T.);
#864=FACE_OUTER_BOUND('',#1240,.T.);
#865=FACE_OUTER_BOUND('',#1241,.T.);
#866=FACE_OUTER_BOUND('',#1242,.T.);
#867=FACE_OUTER_BOUND('',#1243,.T.);
#868=FACE_OUTER_BOUND('',#1244,.T.);
#869=FACE_OUTER_BOUND('',#1245,.T.);
#870=FACE_OUTER_BOUND('',#1246,.T.);
#871=FACE_OUTER_BOUND('',#1247,.T.);
#872=FACE_OUTER_BOUND('',#1248,.T.);
#873=FACE_OUTER_BOUND('',#1249,.T.);
#874=FACE_OUTER_BOUND('',#1250,.T.);
#875=FACE_OUTER_BOUND('',#1251,.T.);
#876=FACE_OUTER_BOUND('',#1252,.T.);
#877=FACE_OUTER_BOUND('',#1253,.T.);
#878=FACE_OUTER_BOUND('',#1254,.T.);
#879=FACE_OUTER_BOUND('',#1255,.T.);
#880=FACE_OUTER_BOUND('',#1256,.T.);
#881=FACE_OUTER_BOUND('',#1257,.T.);
#882=FACE_OUTER_BOUND('',#1258,.T.);
#883=FACE_OUTER_BOUND('',#1259,.T.);
#884=FACE_OUTER_BOUND('',#1260,.T.);
#885=FACE_OUTER_BOUND('',#1261,.T.);
#886=FACE_OUTER_BOUND('',#1262,.T.);
#887=FACE_OUTER_BOUND('',#1264,.T.);
#888=FACE_OUTER_BOUND('',#1265,.T.);
#889=FACE_OUTER_BOUND('',#1267,.T.);
#890=FACE_OUTER_BOUND('',#1268,.T.);
#891=FACE_OUTER_BOUND('',#1270,.T.);
#892=FACE_OUTER_BOUND('',#1271,.T.);
#893=FACE_OUTER_BOUND('',#1273,.T.);
#894=FACE_OUTER_BOUND('',#1274,.T.);
#895=FACE_OUTER_BOUND('',#1276,.T.);
#896=FACE_OUTER_BOUND('',#1277,.T.);
#897=FACE_OUTER_BOUND('',#1278,.T.);
#898=FACE_OUTER_BOUND('',#1279,.T.);
#899=FACE_OUTER_BOUND('',#1280,.T.);
#900=FACE_OUTER_BOUND('',#1281,.T.);
#901=FACE_OUTER_BOUND('',#1282,.T.);
#902=FACE_OUTER_BOUND('',#1284,.T.);
#903=FACE_OUTER_BOUND('',#1286,.T.);
#904=FACE_OUTER_BOUND('',#1287,.T.);
#905=FACE_OUTER_BOUND('',#1289,.T.);
#906=FACE_OUTER_BOUND('',#1290,.T.);
#907=FACE_OUTER_BOUND('',#1291,.T.);
#908=FACE_OUTER_BOUND('',#1292,.T.);
#909=FACE_OUTER_BOUND('',#1293,.T.);
#910=FACE_OUTER_BOUND('',#1294,.T.);
#911=FACE_OUTER_BOUND('',#1295,.T.);
#912=FACE_OUTER_BOUND('',#1296,.T.);
#913=FACE_OUTER_BOUND('',#1297,.T.);
#914=FACE_OUTER_BOUND('',#1298,.T.);
#915=FACE_OUTER_BOUND('',#1299,.T.);
#916=FACE_OUTER_BOUND('',#1300,.T.);
#917=FACE_OUTER_BOUND('',#1302,.T.);
#918=FACE_OUTER_BOUND('',#1304,.T.);
#919=FACE_OUTER_BOUND('',#1305,.T.);
#920=FACE_OUTER_BOUND('',#1306,.T.);
#921=FACE_OUTER_BOUND('',#1310,.T.);
#922=FACE_OUTER_BOUND('',#1311,.T.);
#923=FACE_OUTER_BOUND('',#1312,.T.);
#924=FACE_OUTER_BOUND('',#1313,.T.);
#925=FACE_OUTER_BOUND('',#1314,.T.);
#926=FACE_OUTER_BOUND('',#1315,.T.);
#927=FACE_OUTER_BOUND('',#1316,.T.);
#928=FACE_OUTER_BOUND('',#1320,.T.);
#929=FACE_OUTER_BOUND('',#1321,.T.);
#930=FACE_OUTER_BOUND('',#1322,.T.);
#931=FACE_OUTER_BOUND('',#1327,.T.);
#932=FACE_OUTER_BOUND('',#1329,.T.);
#933=FACE_OUTER_BOUND('',#1330,.T.);
#934=FACE_OUTER_BOUND('',#1331,.T.);
#935=FACE_OUTER_BOUND('',#1333,.T.);
#936=FACE_OUTER_BOUND('',#1335,.T.);
#937=FACE_OUTER_BOUND('',#1336,.T.);
#938=FACE_OUTER_BOUND('',#1337,.T.);
#939=FACE_OUTER_BOUND('',#1338,.T.);
#940=FACE_OUTER_BOUND('',#1340,.T.);
#941=FACE_OUTER_BOUND('',#1342,.T.);
#942=FACE_OUTER_BOUND('',#1344,.T.);
#943=FACE_OUTER_BOUND('',#1346,.T.);
#944=FACE_OUTER_BOUND('',#1347,.T.);
#945=FACE_OUTER_BOUND('',#1348,.T.);
#946=FACE_OUTER_BOUND('',#1349,.T.);
#947=FACE_OUTER_BOUND('',#1350,.T.);
#948=FACE_OUTER_BOUND('',#1354,.T.);
#949=FACE_OUTER_BOUND('',#1355,.T.);
#950=FACE_OUTER_BOUND('',#1357,.T.);
#951=FACE_OUTER_BOUND('',#1358,.T.);
#952=FACE_OUTER_BOUND('',#1359,.T.);
#953=FACE_OUTER_BOUND('',#1362,.T.);
#954=FACE_OUTER_BOUND('',#1364,.T.);
#955=FACE_OUTER_BOUND('',#1365,.T.);
#956=FACE_OUTER_BOUND('',#1366,.T.);
#957=FACE_OUTER_BOUND('',#1368,.T.);
#958=FACE_OUTER_BOUND('',#1370,.T.);
#959=FACE_OUTER_BOUND('',#1371,.T.);
#960=FACE_OUTER_BOUND('',#1372,.T.);
#961=FACE_OUTER_BOUND('',#1374,.T.);
#962=FACE_OUTER_BOUND('',#1376,.T.);
#963=FACE_OUTER_BOUND('',#1377,.T.);
#964=FACE_OUTER_BOUND('',#1378,.T.);
#965=FACE_OUTER_BOUND('',#1379,.T.);
#966=FACE_OUTER_BOUND('',#1380,.T.);
#967=FACE_OUTER_BOUND('',#1381,.T.);
#968=FACE_OUTER_BOUND('',#1382,.T.);
#969=FACE_OUTER_BOUND('',#1383,.T.);
#970=FACE_OUTER_BOUND('',#1384,.T.);
#971=FACE_OUTER_BOUND('',#1385,.T.);
#972=FACE_OUTER_BOUND('',#1386,.T.);
#973=FACE_OUTER_BOUND('',#1387,.T.);
#974=FACE_OUTER_BOUND('',#1388,.T.);
#975=FACE_OUTER_BOUND('',#1389,.T.);
#976=FACE_OUTER_BOUND('',#1390,.T.);
#977=FACE_OUTER_BOUND('',#1391,.T.);
#978=FACE_OUTER_BOUND('',#1392,.T.);
#979=FACE_OUTER_BOUND('',#1393,.T.);
#980=FACE_OUTER_BOUND('',#1394,.T.);
#981=FACE_OUTER_BOUND('',#1395,.T.);
#982=FACE_OUTER_BOUND('',#1396,.T.);
#983=FACE_OUTER_BOUND('',#1397,.T.);
#984=FACE_OUTER_BOUND('',#1399,.T.);
#985=FACE_OUTER_BOUND('',#1400,.T.);
#986=FACE_OUTER_BOUND('',#1401,.T.);
#987=FACE_OUTER_BOUND('',#1402,.T.);
#988=FACE_OUTER_BOUND('',#1403,.T.);
#989=FACE_OUTER_BOUND('',#1404,.T.);
#990=FACE_OUTER_BOUND('',#1405,.T.);
#991=FACE_OUTER_BOUND('',#1406,.T.);
#992=FACE_OUTER_BOUND('',#1407,.T.);
#993=FACE_OUTER_BOUND('',#1408,.T.);
#994=FACE_OUTER_BOUND('',#1409,.T.);
#995=FACE_OUTER_BOUND('',#1410,.T.);
#996=FACE_OUTER_BOUND('',#1411,.T.);
#997=FACE_OUTER_BOUND('',#1412,.T.);
#998=FACE_OUTER_BOUND('',#1413,.T.);
#999=FACE_OUTER_BOUND('',#1414,.T.);
#1000=FACE_OUTER_BOUND('',#1415,.T.);
#1001=FACE_OUTER_BOUND('',#1416,.T.);
#1002=FACE_OUTER_BOUND('',#1418,.T.);
#1003=FACE_OUTER_BOUND('',#1419,.T.);
#1004=FACE_OUTER_BOUND('',#1420,.T.);
#1005=FACE_OUTER_BOUND('',#1421,.T.);
#1006=FACE_OUTER_BOUND('',#1422,.T.);
#1007=FACE_OUTER_BOUND('',#1423,.T.);
#1008=FACE_OUTER_BOUND('',#1424,.T.);
#1009=FACE_OUTER_BOUND('',#1426,.T.);
#1010=FACE_OUTER_BOUND('',#1427,.T.);
#1011=FACE_OUTER_BOUND('',#1429,.T.);
#1012=FACE_OUTER_BOUND('',#1430,.T.);
#1013=FACE_OUTER_BOUND('',#1431,.T.);
#1014=FACE_OUTER_BOUND('',#1432,.T.);
#1015=FACE_OUTER_BOUND('',#1434,.T.);
#1016=FACE_OUTER_BOUND('',#1435,.T.);
#1017=FACE_OUTER_BOUND('',#1436,.T.);
#1018=FACE_OUTER_BOUND('',#1437,.T.);
#1019=FACE_OUTER_BOUND('',#1439,.T.);
#1020=FACE_OUTER_BOUND('',#1440,.T.);
#1021=FACE_OUTER_BOUND('',#1441,.T.);
#1022=FACE_OUTER_BOUND('',#1442,.T.);
#1023=FACE_OUTER_BOUND('',#1443,.T.);
#1024=FACE_OUTER_BOUND('',#1444,.T.);
#1025=FACE_OUTER_BOUND('',#1445,.T.);
#1026=FACE_OUTER_BOUND('',#1446,.T.);
#1027=FACE_OUTER_BOUND('',#1447,.T.);
#1028=FACE_OUTER_BOUND('',#1448,.T.);
#1029=FACE_OUTER_BOUND('',#1449,.T.);
#1030=FACE_OUTER_BOUND('',#1450,.T.);
#1031=FACE_OUTER_BOUND('',#1451,.T.);
#1032=FACE_OUTER_BOUND('',#1452,.T.);
#1033=FACE_OUTER_BOUND('',#1453,.T.);
#1034=FACE_OUTER_BOUND('',#1454,.T.);
#1035=FACE_OUTER_BOUND('',#1455,.T.);
#1036=FACE_OUTER_BOUND('',#1456,.T.);
#1037=FACE_OUTER_BOUND('',#1457,.T.);
#1038=FACE_OUTER_BOUND('',#1458,.T.);
#1039=FACE_OUTER_BOUND('',#1459,.T.);
#1040=FACE_OUTER_BOUND('',#1460,.T.);
#1041=FACE_OUTER_BOUND('',#1461,.T.);
#1042=FACE_OUTER_BOUND('',#1462,.T.);
#1043=FACE_OUTER_BOUND('',#1463,.T.);
#1044=FACE_OUTER_BOUND('',#1464,.T.);
#1045=FACE_OUTER_BOUND('',#1465,.T.);
#1046=FACE_OUTER_BOUND('',#1467,.T.);
#1047=FACE_OUTER_BOUND('',#1468,.T.);
#1048=FACE_OUTER_BOUND('',#1470,.T.);
#1049=FACE_OUTER_BOUND('',#1471,.T.);
#1050=FACE_OUTER_BOUND('',#1473,.T.);
#1051=FACE_OUTER_BOUND('',#1474,.T.);
#1052=FACE_OUTER_BOUND('',#1476,.T.);
#1053=FACE_OUTER_BOUND('',#1477,.T.);
#1054=FACE_OUTER_BOUND('',#1479,.T.);
#1055=FACE_OUTER_BOUND('',#1480,.T.);
#1056=FACE_OUTER_BOUND('',#1481,.T.);
#1057=FACE_OUTER_BOUND('',#1482,.T.);
#1058=FACE_OUTER_BOUND('',#1483,.T.);
#1059=FACE_OUTER_BOUND('',#1484,.T.);
#1060=FACE_OUTER_BOUND('',#1486,.T.);
#1061=FACE_OUTER_BOUND('',#1487,.T.);
#1062=FACE_OUTER_BOUND('',#1488,.T.);
#1063=FACE_OUTER_BOUND('',#1489,.T.);
#1064=FACE_OUTER_BOUND('',#1490,.T.);
#1065=FACE_OUTER_BOUND('',#1491,.T.);
#1066=FACE_OUTER_BOUND('',#1492,.T.);
#1067=FACE_OUTER_BOUND('',#1493,.T.);
#1068=FACE_OUTER_BOUND('',#1494,.T.);
#1069=FACE_OUTER_BOUND('',#1495,.T.);
#1070=FACE_OUTER_BOUND('',#1496,.T.);
#1071=FACE_OUTER_BOUND('',#1497,.T.);
#1072=FACE_OUTER_BOUND('',#1498,.T.);
#1073=FACE_OUTER_BOUND('',#1499,.T.);
#1074=FACE_OUTER_BOUND('',#1501,.T.);
#1075=FACE_OUTER_BOUND('',#1502,.T.);
#1076=FACE_OUTER_BOUND('',#1503,.T.);
#1077=FACE_OUTER_BOUND('',#1505,.T.);
#1078=FACE_OUTER_BOUND('',#1507,.T.);
#1079=FACE_OUTER_BOUND('',#1508,.T.);
#1080=FACE_OUTER_BOUND('',#1509,.T.);
#1081=FACE_OUTER_BOUND('',#1511,.T.);
#1082=EDGE_LOOP('',(#3557,#3558,#3559,#3560));
#1083=EDGE_LOOP('',(#3561,#3562,#3563,#3564));
#1084=EDGE_LOOP('',(#3565,#3566,#3567,#3568));
#1085=EDGE_LOOP('',(#3569,#3570,#3571,#3572));
#1086=EDGE_LOOP('',(#3573,#3574,#3575,#3576));
#1087=EDGE_LOOP('',(#3577,#3578,#3579,#3580));
#1088=EDGE_LOOP('',(#3581,#3582,#3583,#3584));
#1089=EDGE_LOOP('',(#3585,#3586,#3587,#3588));
#1090=EDGE_LOOP('',(#3589,#3590,#3591,#3592));
#1091=EDGE_LOOP('',(#3593));
#1092=EDGE_LOOP('',(#3594));
#1093=EDGE_LOOP('',(#3595));
#1094=EDGE_LOOP('',(#3596));
#1095=EDGE_LOOP('',(#3597,#3598,#3599,#3600));
#1096=EDGE_LOOP('',(#3601));
#1097=EDGE_LOOP('',(#3602));
#1098=EDGE_LOOP('',(#3603));
#1099=EDGE_LOOP('',(#3604));
#1100=EDGE_LOOP('',(#3605,#3606,#3607,#3608));
#1101=EDGE_LOOP('',(#3609,#3610,#3611,#3612));
#1102=EDGE_LOOP('',(#3613,#3614,#3615,#3616));
#1103=EDGE_LOOP('',(#3617,#3618,#3619,#3620));
#1104=EDGE_LOOP('',(#3621,#3622,#3623,#3624));
#1105=EDGE_LOOP('',(#3625,#3626,#3627,#3628));
#1106=EDGE_LOOP('',(#3629,#3630,#3631,#3632));
#1107=EDGE_LOOP('',(#3633,#3634,#3635,#3636));
#1108=EDGE_LOOP('',(#3637,#3638,#3639,#3640));
#1109=EDGE_LOOP('',(#3641,#3642,#3643,#3644));
#1110=EDGE_LOOP('',(#3645,#3646,#3647,#3648));
#1111=EDGE_LOOP('',(#3649,#3650,#3651,#3652));
#1112=EDGE_LOOP('',(#3653,#3654,#3655,#3656));
#1113=EDGE_LOOP('',(#3657,#3658,#3659,#3660));
#1114=EDGE_LOOP('',(#3661,#3662,#3663,#3664));
#1115=EDGE_LOOP('',(#3665,#3666,#3667,#3668));
#1116=EDGE_LOOP('',(#3669,#3670,#3671,#3672));
#1117=EDGE_LOOP('',(#3673,#3674,#3675,#3676));
#1118=EDGE_LOOP('',(#3677,#3678,#3679,#3680));
#1119=EDGE_LOOP('',(#3681,#3682,#3683,#3684));
#1120=EDGE_LOOP('',(#3685,#3686,#3687,#3688));
#1121=EDGE_LOOP('',(#3689,#3690,#3691,#3692));
#1122=EDGE_LOOP('',(#3693));
#1123=EDGE_LOOP('',(#3694));
#1124=EDGE_LOOP('',(#3695,#3696,#3697,#3698));
#1125=EDGE_LOOP('',(#3699));
#1126=EDGE_LOOP('',(#3700));
#1127=EDGE_LOOP('',(#3701,#3702,#3703,#3704));
#1128=EDGE_LOOP('',(#3705,#3706,#3707,#3708));
#1129=EDGE_LOOP('',(#3709,#3710,#3711,#3712,#3713,#3714,#3715,#3716));
#1130=EDGE_LOOP('',(#3717));
#1131=EDGE_LOOP('',(#3718));
#1132=EDGE_LOOP('',(#3719));
#1133=EDGE_LOOP('',(#3720));
#1134=EDGE_LOOP('',(#3721));
#1135=EDGE_LOOP('',(#3722,#3723,#3724,#3725));
#1136=EDGE_LOOP('',(#3726,#3727,#3728,#3729,#3730,#3731,#3732,#3733));
#1137=EDGE_LOOP('',(#3734));
#1138=EDGE_LOOP('',(#3735));
#1139=EDGE_LOOP('',(#3736));
#1140=EDGE_LOOP('',(#3737));
#1141=EDGE_LOOP('',(#3738));
#1142=EDGE_LOOP('',(#3739,#3740,#3741,#3742));
#1143=EDGE_LOOP('',(#3743,#3744,#3745,#3746));
#1144=EDGE_LOOP('',(#3747,#3748,#3749,#3750));
#1145=EDGE_LOOP('',(#3751));
#1146=EDGE_LOOP('',(#3752));
#1147=EDGE_LOOP('',(#3753));
#1148=EDGE_LOOP('',(#3754));
#1149=EDGE_LOOP('',(#3755,#3756,#3757,#3758));
#1150=EDGE_LOOP('',(#3759,#3760,#3761,#3762));
#1151=EDGE_LOOP('',(#3763));
#1152=EDGE_LOOP('',(#3764));
#1153=EDGE_LOOP('',(#3765));
#1154=EDGE_LOOP('',(#3766));
#1155=EDGE_LOOP('',(#3767,#3768,#3769,#3770));
#1156=EDGE_LOOP('',(#3771,#3772,#3773,#3774));
#1157=EDGE_LOOP('',(#3775,#3776,#3777,#3778));
#1158=EDGE_LOOP('',(#3779,#3780,#3781,#3782));
#1159=EDGE_LOOP('',(#3783,#3784,#3785,#3786));
#1160=EDGE_LOOP('',(#3787));
#1161=EDGE_LOOP('',(#3788));
#1162=EDGE_LOOP('',(#3789,#3790,#3791,#3792));
#1163=EDGE_LOOP('',(#3793,#3794,#3795,#3796));
#1164=EDGE_LOOP('',(#3797));
#1165=EDGE_LOOP('',(#3798));
#1166=EDGE_LOOP('',(#3799));
#1167=EDGE_LOOP('',(#3800));
#1168=EDGE_LOOP('',(#3801));
#1169=EDGE_LOOP('',(#3802));
#1170=EDGE_LOOP('',(#3803));
#1171=EDGE_LOOP('',(#3804));
#1172=EDGE_LOOP('',(#3805));
#1173=EDGE_LOOP('',(#3806));
#1174=EDGE_LOOP('',(#3807));
#1175=EDGE_LOOP('',(#3808));
#1176=EDGE_LOOP('',(#3809,#3810,#3811,#3812));
#1177=EDGE_LOOP('',(#3813,#3814,#3815,#3816));
#1178=EDGE_LOOP('',(#3817,#3818,#3819,#3820));
#1179=EDGE_LOOP('',(#3821,#3822,#3823,#3824));
#1180=EDGE_LOOP('',(#3825,#3826,#3827,#3828));
#1181=EDGE_LOOP('',(#3829));
#1182=EDGE_LOOP('',(#3830));
#1183=EDGE_LOOP('',(#3831,#3832,#3833,#3834));
#1184=EDGE_LOOP('',(#3835,#3836,#3837,#3838));
#1185=EDGE_LOOP('',(#3839));
#1186=EDGE_LOOP('',(#3840));
#1187=EDGE_LOOP('',(#3841));
#1188=EDGE_LOOP('',(#3842));
#1189=EDGE_LOOP('',(#3843));
#1190=EDGE_LOOP('',(#3844));
#1191=EDGE_LOOP('',(#3845));
#1192=EDGE_LOOP('',(#3846));
#1193=EDGE_LOOP('',(#3847));
#1194=EDGE_LOOP('',(#3848));
#1195=EDGE_LOOP('',(#3849));
#1196=EDGE_LOOP('',(#3850));
#1197=EDGE_LOOP('',(#3851,#3852,#3853,#3854));
#1198=EDGE_LOOP('',(#3855,#3856,#3857,#3858));
#1199=EDGE_LOOP('',(#3859));
#1200=EDGE_LOOP('',(#3860));
#1201=EDGE_LOOP('',(#3861));
#1202=EDGE_LOOP('',(#3862));
#1203=EDGE_LOOP('',(#3863,#3864,#3865,#3866));
#1204=EDGE_LOOP('',(#3867,#3868,#3869,#3870));
#1205=EDGE_LOOP('',(#3871,#3872,#3873,#3874));
#1206=EDGE_LOOP('',(#3875,#3876,#3877,#3878));
#1207=EDGE_LOOP('',(#3879,#3880,#3881,#3882));
#1208=EDGE_LOOP('',(#3883,#3884,#3885,#3886));
#1209=EDGE_LOOP('',(#3887,#3888,#3889,#3890,#3891,#3892));
#1210=EDGE_LOOP('',(#3893,#3894,#3895,#3896,#3897,#3898));
#1211=EDGE_LOOP('',(#3899));
#1212=EDGE_LOOP('',(#3900));
#1213=EDGE_LOOP('',(#3901,#3902,#3903,#3904));
#1214=EDGE_LOOP('',(#3905,#3906,#3907,#3908));
#1215=EDGE_LOOP('',(#3909,#3910,#3911,#3912));
#1216=EDGE_LOOP('',(#3913));
#1217=EDGE_LOOP('',(#3914));
#1218=EDGE_LOOP('',(#3915,#3916,#3917,#3918));
#1219=EDGE_LOOP('',(#3919,#3920,#3921,#3922));
#1220=EDGE_LOOP('',(#3923,#3924,#3925,#3926,#3927,#3928));
#1221=EDGE_LOOP('',(#3929,#3930,#3931,#3932,#3933));
#1222=EDGE_LOOP('',(#3934,#3935,#3936,#3937));
#1223=EDGE_LOOP('',(#3938,#3939,#3940,#3941));
#1224=EDGE_LOOP('',(#3942));
#1225=EDGE_LOOP('',(#3943));
#1226=EDGE_LOOP('',(#3944,#3945,#3946,#3947,#3948));
#1227=EDGE_LOOP('',(#3949));
#1228=EDGE_LOOP('',(#3950));
#1229=EDGE_LOOP('',(#3951,#3952,#3953,#3954));
#1230=EDGE_LOOP('',(#3955,#3956,#3957,#3958,#3959,#3960));
#1231=EDGE_LOOP('',(#3961,#3962,#3963,#3964,#3965));
#1232=EDGE_LOOP('',(#3966));
#1233=EDGE_LOOP('',(#3967));
#1234=EDGE_LOOP('',(#3968,#3969,#3970,#3971));
#1235=EDGE_LOOP('',(#3972,#3973,#3974,#3975));
#1236=EDGE_LOOP('',(#3976,#3977,#3978,#3979));
#1237=EDGE_LOOP('',(#3980));
#1238=EDGE_LOOP('',(#3981));
#1239=EDGE_LOOP('',(#3982,#3983,#3984,#3985,#3986));
#1240=EDGE_LOOP('',(#3987,#3988));
#1241=EDGE_LOOP('',(#3989,#3990));
#1242=EDGE_LOOP('',(#3991,#3992));
#1243=EDGE_LOOP('',(#3993,#3994));
#1244=EDGE_LOOP('',(#3995,#3996));
#1245=EDGE_LOOP('',(#3997,#3998));
#1246=EDGE_LOOP('',(#3999,#4000));
#1247=EDGE_LOOP('',(#4001,#4002,#4003,#4004));
#1248=EDGE_LOOP('',(#4005,#4006,#4007,#4008,#4009,#4010,#4011,#4012,#4013,
#4014,#4015,#4016,#4017,#4018,#4019,#4020,#4021,#4022));
#1249=EDGE_LOOP('',(#4023,#4024,#4025,#4026));
#1250=EDGE_LOOP('',(#4027,#4028,#4029,#4030));
#1251=EDGE_LOOP('',(#4031,#4032,#4033,#4034));
#1252=EDGE_LOOP('',(#4035,#4036,#4037,#4038));
#1253=EDGE_LOOP('',(#4039,#4040,#4041,#4042,#4043,#4044));
#1254=EDGE_LOOP('',(#4045,#4046,#4047,#4048));
#1255=EDGE_LOOP('',(#4049,#4050,#4051,#4052));
#1256=EDGE_LOOP('',(#4053,#4054,#4055,#4056));
#1257=EDGE_LOOP('',(#4057,#4058,#4059,#4060));
#1258=EDGE_LOOP('',(#4061,#4062,#4063,#4064));
#1259=EDGE_LOOP('',(#4065,#4066,#4067,#4068,#4069,#4070,#4071,#4072,#4073,
#4074,#4075,#4076,#4077,#4078,#4079,#4080,#4081,#4082));
#1260=EDGE_LOOP('',(#4083,#4084,#4085,#4086));
#1261=EDGE_LOOP('',(#4087,#4088,#4089,#4090));
#1262=EDGE_LOOP('',(#4091));
#1263=EDGE_LOOP('',(#4092));
#1264=EDGE_LOOP('',(#4093,#4094,#4095,#4096));
#1265=EDGE_LOOP('',(#4097));
#1266=EDGE_LOOP('',(#4098));
#1267=EDGE_LOOP('',(#4099,#4100,#4101,#4102));
#1268=EDGE_LOOP('',(#4103));
#1269=EDGE_LOOP('',(#4104));
#1270=EDGE_LOOP('',(#4105,#4106,#4107,#4108));
#1271=EDGE_LOOP('',(#4109));
#1272=EDGE_LOOP('',(#4110));
#1273=EDGE_LOOP('',(#4111,#4112,#4113,#4114));
#1274=EDGE_LOOP('',(#4115));
#1275=EDGE_LOOP('',(#4116));
#1276=EDGE_LOOP('',(#4117,#4118,#4119,#4120));
#1277=EDGE_LOOP('',(#4121,#4122,#4123,#4124));
#1278=EDGE_LOOP('',(#4125,#4126,#4127,#4128));
#1279=EDGE_LOOP('',(#4129,#4130,#4131,#4132));
#1280=EDGE_LOOP('',(#4133,#4134,#4135,#4136));
#1281=EDGE_LOOP('',(#4137,#4138,#4139,#4140));
#1282=EDGE_LOOP('',(#4141));
#1283=EDGE_LOOP('',(#4142));
#1284=EDGE_LOOP('',(#4143));
#1285=EDGE_LOOP('',(#4144));
#1286=EDGE_LOOP('',(#4145,#4146,#4147,#4148));
#1287=EDGE_LOOP('',(#4149,#4150,#4151,#4152));
#1288=EDGE_LOOP('',(#4153,#4154,#4155,#4156));
#1289=EDGE_LOOP('',(#4157,#4158,#4159,#4160));
#1290=EDGE_LOOP('',(#4161));
#1291=EDGE_LOOP('',(#4162));
#1292=EDGE_LOOP('',(#4163,#4164,#4165,#4166));
#1293=EDGE_LOOP('',(#4167,#4168,#4169,#4170));
#1294=EDGE_LOOP('',(#4171,#4172));
#1295=EDGE_LOOP('',(#4173,#4174,#4175,#4176,#4177,#4178,#4179,#4180,#4181));
#1296=EDGE_LOOP('',(#4182,#4183,#4184));
#1297=EDGE_LOOP('',(#4185,#4186,#4187,#4188));
#1298=EDGE_LOOP('',(#4189,#4190,#4191,#4192));
#1299=EDGE_LOOP('',(#4193,#4194,#4195,#4196));
#1300=EDGE_LOOP('',(#4197));
#1301=EDGE_LOOP('',(#4198,#4199,#4200,#4201));
#1302=EDGE_LOOP('',(#4202,#4203,#4204,#4205));
#1303=EDGE_LOOP('',(#4206,#4207,#4208,#4209));
#1304=EDGE_LOOP('',(#4210,#4211,#4212,#4213));
#1305=EDGE_LOOP('',(#4214,#4215,#4216,#4217));
#1306=EDGE_LOOP('',(#4218));
#1307=EDGE_LOOP('',(#4219));
#1308=EDGE_LOOP('',(#4220));
#1309=EDGE_LOOP('',(#4221,#4222,#4223,#4224,#4225,#4226,#4227,#4228,#4229,
#4230,#4231,#4232));
#1310=EDGE_LOOP('',(#4233,#4234,#4235,#4236));
#1311=EDGE_LOOP('',(#4237,#4238,#4239,#4240));
#1312=EDGE_LOOP('',(#4241,#4242,#4243,#4244));
#1313=EDGE_LOOP('',(#4245,#4246,#4247,#4248));
#1314=EDGE_LOOP('',(#4249,#4250,#4251,#4252));
#1315=EDGE_LOOP('',(#4253,#4254,#4255,#4256));
#1316=EDGE_LOOP('',(#4257));
#1317=EDGE_LOOP('',(#4258));
#1318=EDGE_LOOP('',(#4259));
#1319=EDGE_LOOP('',(#4260,#4261,#4262,#4263,#4264,#4265,#4266,#4267,#4268,
#4269,#4270,#4271));
#1320=EDGE_LOOP('',(#4272,#4273,#4274,#4275));
#1321=EDGE_LOOP('',(#4276,#4277,#4278,#4279));
#1322=EDGE_LOOP('',(#4280,#4281,#4282,#4283));
#1323=EDGE_LOOP('',(#4284,#4285));
#1324=EDGE_LOOP('',(#4286,#4287,#4288,#4289));
#1325=EDGE_LOOP('',(#4290,#4291,#4292,#4293));
#1326=EDGE_LOOP('',(#4294,#4295,#4296,#4297));
#1327=EDGE_LOOP('',(#4298));
#1328=EDGE_LOOP('',(#4299,#4300,#4301,#4302));
#1329=EDGE_LOOP('',(#4303,#4304,#4305,#4306));
#1330=EDGE_LOOP('',(#4307,#4308,#4309,#4310));
#1331=EDGE_LOOP('',(#4311));
#1332=EDGE_LOOP('',(#4312));
#1333=EDGE_LOOP('',(#4313));
#1334=EDGE_LOOP('',(#4314));
#1335=EDGE_LOOP('',(#4315,#4316));
#1336=EDGE_LOOP('',(#4317,#4318,#4319,#4320,#4321,#4322,#4323,#4324,#4325));
#1337=EDGE_LOOP('',(#4326,#4327,#4328));
#1338=EDGE_LOOP('',(#4329,#4330,#4331,#4332));
#1339=EDGE_LOOP('',(#4333,#4334,#4335,#4336));
#1340=EDGE_LOOP('',(#4337,#4338,#4339,#4340));
#1341=EDGE_LOOP('',(#4341,#4342));
#1342=EDGE_LOOP('',(#4343));
#1343=EDGE_LOOP('',(#4344));
#1344=EDGE_LOOP('',(#4345));
#1345=EDGE_LOOP('',(#4346));
#1346=EDGE_LOOP('',(#4347,#4348,#4349,#4350));
#1347=EDGE_LOOP('',(#4351));
#1348=EDGE_LOOP('',(#4352,#4353,#4354,#4355));
#1349=EDGE_LOOP('',(#4356,#4357,#4358,#4359));
#1350=EDGE_LOOP('',(#4360));
#1351=EDGE_LOOP('',(#4361));
#1352=EDGE_LOOP('',(#4362));
#1353=EDGE_LOOP('',(#4363));
#1354=EDGE_LOOP('',(#4364,#4365,#4366,#4367));
#1355=EDGE_LOOP('',(#4368));
#1356=EDGE_LOOP('',(#4369));
#1357=EDGE_LOOP('',(#4370,#4371,#4372,#4373));
#1358=EDGE_LOOP('',(#4374,#4375,#4376,#4377));
#1359=EDGE_LOOP('',(#4378));
#1360=EDGE_LOOP('',(#4379));
#1361=EDGE_LOOP('',(#4380));
#1362=EDGE_LOOP('',(#4381));
#1363=EDGE_LOOP('',(#4382));
#1364=EDGE_LOOP('',(#4383,#4384,#4385,#4386));
#1365=EDGE_LOOP('',(#4387,#4388,#4389,#4390));
#1366=EDGE_LOOP('',(#4391));
#1367=EDGE_LOOP('',(#4392));
#1368=EDGE_LOOP('',(#4393));
#1369=EDGE_LOOP('',(#4394));
#1370=EDGE_LOOP('',(#4395,#4396,#4397,#4398));
#1371=EDGE_LOOP('',(#4399,#4400,#4401,#4402));
#1372=EDGE_LOOP('',(#4403));
#1373=EDGE_LOOP('',(#4404));
#1374=EDGE_LOOP('',(#4405));
#1375=EDGE_LOOP('',(#4406));
#1376=EDGE_LOOP('',(#4407,#4408,#4409,#4410));
#1377=EDGE_LOOP('',(#4411,#4412,#4413,#4414));
#1378=EDGE_LOOP('',(#4415,#4416,#4417,#4418));
#1379=EDGE_LOOP('',(#4419,#4420,#4421,#4422));
#1380=EDGE_LOOP('',(#4423,#4424,#4425,#4426));
#1381=EDGE_LOOP('',(#4427,#4428,#4429,#4430));
#1382=EDGE_LOOP('',(#4431,#4432,#4433,#4434));
#1383=EDGE_LOOP('',(#4435,#4436,#4437,#4438));
#1384=EDGE_LOOP('',(#4439,#4440,#4441,#4442));
#1385=EDGE_LOOP('',(#4443,#4444,#4445,#4446));
#1386=EDGE_LOOP('',(#4447,#4448,#4449,#4450));
#1387=EDGE_LOOP('',(#4451,#4452,#4453,#4454));
#1388=EDGE_LOOP('',(#4455,#4456,#4457,#4458));
#1389=EDGE_LOOP('',(#4459,#4460,#4461,#4462));
#1390=EDGE_LOOP('',(#4463,#4464,#4465,#4466));
#1391=EDGE_LOOP('',(#4467,#4468,#4469,#4470));
#1392=EDGE_LOOP('',(#4471,#4472,#4473,#4474));
#1393=EDGE_LOOP('',(#4475,#4476,#4477,#4478));
#1394=EDGE_LOOP('',(#4479,#4480,#4481,#4482));
#1395=EDGE_LOOP('',(#4483,#4484,#4485,#4486));
#1396=EDGE_LOOP('',(#4487,#4488,#4489,#4490,#4491,#4492));
#1397=EDGE_LOOP('',(#4493));
#1398=EDGE_LOOP('',(#4494,#4495,#4496,#4497,#4498,#4499));
#1399=EDGE_LOOP('',(#4500,#4501,#4502,#4503));
#1400=EDGE_LOOP('',(#4504,#4505,#4506,#4507));
#1401=EDGE_LOOP('',(#4508,#4509,#4510,#4511));
#1402=EDGE_LOOP('',(#4512));
#1403=EDGE_LOOP('',(#4513,#4514,#4515,#4516));
#1404=EDGE_LOOP('',(#4517,#4518,#4519,#4520));
#1405=EDGE_LOOP('',(#4521,#4522,#4523,#4524));
#1406=EDGE_LOOP('',(#4525,#4526,#4527,#4528));
#1407=EDGE_LOOP('',(#4529,#4530,#4531,#4532));
#1408=EDGE_LOOP('',(#4533,#4534,#4535,#4536));
#1409=EDGE_LOOP('',(#4537,#4538,#4539,#4540,#4541,#4542));
#1410=EDGE_LOOP('',(#4543,#4544,#4545,#4546,#4547,#4548));
#1411=EDGE_LOOP('',(#4549));
#1412=EDGE_LOOP('',(#4550));
#1413=EDGE_LOOP('',(#4551,#4552,#4553,#4554));
#1414=EDGE_LOOP('',(#4555,#4556,#4557,#4558));
#1415=EDGE_LOOP('',(#4559,#4560,#4561,#4562));
#1416=EDGE_LOOP('',(#4563));
#1417=EDGE_LOOP('',(#4564));
#1418=EDGE_LOOP('',(#4565,#4566,#4567,#4568));
#1419=EDGE_LOOP('',(#4569,#4570,#4571,#4572));
#1420=EDGE_LOOP('',(#4573,#4574,#4575,#4576,#4577,#4578));
#1421=EDGE_LOOP('',(#4579,#4580,#4581,#4582,#4583));
#1422=EDGE_LOOP('',(#4584,#4585,#4586,#4587));
#1423=EDGE_LOOP('',(#4588,#4589,#4590,#4591));
#1424=EDGE_LOOP('',(#4592));
#1425=EDGE_LOOP('',(#4593));
#1426=EDGE_LOOP('',(#4594,#4595,#4596,#4597,#4598));
#1427=EDGE_LOOP('',(#4599));
#1428=EDGE_LOOP('',(#4600));
#1429=EDGE_LOOP('',(#4601,#4602,#4603,#4604));
#1430=EDGE_LOOP('',(#4605,#4606,#4607,#4608,#4609,#4610));
#1431=EDGE_LOOP('',(#4611,#4612,#4613,#4614,#4615));
#1432=EDGE_LOOP('',(#4616));
#1433=EDGE_LOOP('',(#4617));
#1434=EDGE_LOOP('',(#4618,#4619,#4620,#4621));
#1435=EDGE_LOOP('',(#4622,#4623,#4624,#4625));
#1436=EDGE_LOOP('',(#4626,#4627,#4628,#4629));
#1437=EDGE_LOOP('',(#4630));
#1438=EDGE_LOOP('',(#4631));
#1439=EDGE_LOOP('',(#4632,#4633,#4634,#4635,#4636));
#1440=EDGE_LOOP('',(#4637,#4638));
#1441=EDGE_LOOP('',(#4639,#4640));
#1442=EDGE_LOOP('',(#4641,#4642));
#1443=EDGE_LOOP('',(#4643,#4644));
#1444=EDGE_LOOP('',(#4645,#4646));
#1445=EDGE_LOOP('',(#4647,#4648));
#1446=EDGE_LOOP('',(#4649,#4650));
#1447=EDGE_LOOP('',(#4651,#4652));
#1448=EDGE_LOOP('',(#4653,#4654,#4655,#4656));
#1449=EDGE_LOOP('',(#4657,#4658,#4659,#4660,#4661,#4662,#4663,#4664,#4665,
#4666,#4667,#4668,#4669,#4670,#4671,#4672,#4673,#4674,#4675,#4676));
#1450=EDGE_LOOP('',(#4677,#4678,#4679,#4680));
#1451=EDGE_LOOP('',(#4681,#4682,#4683,#4684));
#1452=EDGE_LOOP('',(#4685,#4686,#4687,#4688));
#1453=EDGE_LOOP('',(#4689,#4690,#4691,#4692));
#1454=EDGE_LOOP('',(#4693,#4694,#4695,#4696));
#1455=EDGE_LOOP('',(#4697,#4698,#4699,#4700,#4701,#4702));
#1456=EDGE_LOOP('',(#4703,#4704,#4705,#4706));
#1457=EDGE_LOOP('',(#4707,#4708,#4709,#4710));
#1458=EDGE_LOOP('',(#4711,#4712,#4713,#4714));
#1459=EDGE_LOOP('',(#4715,#4716,#4717,#4718));
#1460=EDGE_LOOP('',(#4719,#4720,#4721,#4722));
#1461=EDGE_LOOP('',(#4723,#4724,#4725,#4726));
#1462=EDGE_LOOP('',(#4727,#4728,#4729,#4730,#4731,#4732,#4733,#4734,#4735,
#4736,#4737,#4738,#4739,#4740,#4741,#4742,#4743,#4744,#4745,#4746));
#1463=EDGE_LOOP('',(#4747,#4748,#4749,#4750));
#1464=EDGE_LOOP('',(#4751,#4752,#4753,#4754));
#1465=EDGE_LOOP('',(#4755));
#1466=EDGE_LOOP('',(#4756));
#1467=EDGE_LOOP('',(#4757,#4758,#4759,#4760));
#1468=EDGE_LOOP('',(#4761));
#1469=EDGE_LOOP('',(#4762));
#1470=EDGE_LOOP('',(#4763,#4764,#4765,#4766));
#1471=EDGE_LOOP('',(#4767));
#1472=EDGE_LOOP('',(#4768));
#1473=EDGE_LOOP('',(#4769,#4770,#4771,#4772));
#1474=EDGE_LOOP('',(#4773));
#1475=EDGE_LOOP('',(#4774));
#1476=EDGE_LOOP('',(#4775,#4776,#4777,#4778));
#1477=EDGE_LOOP('',(#4779));
#1478=EDGE_LOOP('',(#4780));
#1479=EDGE_LOOP('',(#4781,#4782,#4783,#4784));
#1480=EDGE_LOOP('',(#4785));
#1481=EDGE_LOOP('',(#4786,#4787,#4788,#4789));
#1482=EDGE_LOOP('',(#4790,#4791,#4792,#4793));
#1483=EDGE_LOOP('',(#4794,#4795,#4796,#4797));
#1484=EDGE_LOOP('',(#4798));
#1485=EDGE_LOOP('',(#4799));
#1486=EDGE_LOOP('',(#4800,#4801,#4802,#4803));
#1487=EDGE_LOOP('',(#4804,#4805,#4806,#4807));
#1488=EDGE_LOOP('',(#4808,#4809,#4810,#4811));
#1489=EDGE_LOOP('',(#4812));
#1490=EDGE_LOOP('',(#4813,#4814,#4815,#4816));
#1491=EDGE_LOOP('',(#4817,#4818,#4819,#4820));
#1492=EDGE_LOOP('',(#4821,#4822,#4823,#4824));
#1493=EDGE_LOOP('',(#4825,#4826,#4827,#4828));
#1494=EDGE_LOOP('',(#4829,#4830,#4831,#4832));
#1495=EDGE_LOOP('',(#4833,#4834,#4835,#4836));
#1496=EDGE_LOOP('',(#4837,#4838,#4839,#4840,#4841,#4842));
#1497=EDGE_LOOP('',(#4843,#4844,#4845,#4846,#4847,#4848));
#1498=EDGE_LOOP('',(#4849,#4850,#4851,#4852));
#1499=EDGE_LOOP('',(#4853));
#1500=EDGE_LOOP('',(#4854));
#1501=EDGE_LOOP('',(#4855,#4856,#4857,#4858));
#1502=EDGE_LOOP('',(#4859,#4860,#4861,#4862));
#1503=EDGE_LOOP('',(#4863));
#1504=EDGE_LOOP('',(#4864));
#1505=EDGE_LOOP('',(#4865));
#1506=EDGE_LOOP('',(#4866));
#1507=EDGE_LOOP('',(#4867,#4868,#4869,#4870));
#1508=EDGE_LOOP('',(#4871,#4872,#4873,#4874));
#1509=EDGE_LOOP('',(#4875));
#1510=EDGE_LOOP('',(#4876));
#1511=EDGE_LOOP('',(#4877));
#1512=EDGE_LOOP('',(#4878));
#1513=LINE('',#8180,#1823);
#1514=LINE('',#8186,#1824);
#1515=LINE('',#8192,#1825);
#1516=LINE('',#8198,#1826);
#1517=LINE('',#8203,#1827);
#1518=LINE('',#8205,#1828);
#1519=LINE('',#8207,#1829);
#1520=LINE('',#8208,#1830);
#1521=LINE('',#8211,#1831);
#1522=LINE('',#8213,#1832);
#1523=LINE('',#8214,#1833);
#1524=LINE('',#8217,#1834);
#1525=LINE('',#8219,#1835);
#1526=LINE('',#8220,#1836);
#1527=LINE('',#8222,#1837);
#1528=LINE('',#8223,#1838);
#1529=LINE('',#8230,#1839);
#1530=LINE('',#8232,#1840);
#1531=LINE('',#8234,#1841);
#1532=LINE('',#8235,#1842);
#1533=LINE('',#8238,#1843);
#1534=LINE('',#8240,#1844);
#1535=LINE('',#8241,#1845);
#1536=LINE('',#8244,#1846);
#1537=LINE('',#8246,#1847);
#1538=LINE('',#8247,#1848);
#1539=LINE('',#8249,#1849);
#1540=LINE('',#8250,#1850);
#1541=LINE('',#8257,#1851);
#1542=LINE('',#8259,#1852);
#1543=LINE('',#8261,#1853);
#1544=LINE('',#8262,#1854);
#1545=LINE('',#8265,#1855);
#1546=LINE('',#8267,#1856);
#1547=LINE('',#8268,#1857);
#1548=LINE('',#8271,#1858);
#1549=LINE('',#8273,#1859);
#1550=LINE('',#8274,#1860);
#1551=LINE('',#8276,#1861);
#1552=LINE('',#8277,#1862);
#1553=LINE('',#8285,#1863);
#1554=LINE('',#8291,#1864);
#1555=LINE('',#8297,#1865);
#1556=LINE('',#8303,#1866);
#1557=LINE('',#8309,#1867);
#1558=LINE('',#8315,#1868);
#1559=LINE('',#8321,#1869);
#1560=LINE('',#8327,#1870);
#1561=LINE('',#8333,#1871);
#1562=LINE('',#8338,#1872);
#1563=LINE('',#8340,#1873);
#1564=LINE('',#8342,#1874);
#1565=LINE('',#8343,#1875);
#1566=LINE('',#8347,#1876);
#1567=LINE('',#8349,#1877);
#1568=LINE('',#8351,#1878);
#1569=LINE('',#8352,#1879);
#1570=LINE('',#8355,#1880);
#1571=LINE('',#8357,#1881);
#1572=LINE('',#8358,#1882);
#1573=LINE('',#8361,#1883);
#1574=LINE('',#8363,#1884);
#1575=LINE('',#8364,#1885);
#1576=LINE('',#8367,#1886);
#1577=LINE('',#8369,#1887);
#1578=LINE('',#8370,#1888);
#1579=LINE('',#8371,#1889);
#1580=LINE('',#8374,#1890);
#1581=LINE('',#8375,#1891);
#1582=LINE('',#8378,#1892);
#1583=LINE('',#8379,#1893);
#1584=LINE('',#8380,#1894);
#1585=LINE('',#8382,#1895);
#1586=LINE('',#8390,#1896);
#1587=LINE('',#8396,#1897);
#1588=LINE('',#8405,#1898);
#1589=LINE('',#8411,#1899);
#1590=LINE('',#8417,#1900);
#1591=LINE('',#8423,#1901);
#1592=LINE('',#8429,#1902);
#1593=LINE('',#8436,#1903);
#1594=LINE('',#8442,#1904);
#1595=LINE('',#8451,#1905);
#1596=LINE('',#8457,#1906);
#1597=LINE('',#8463,#1907);
#1598=LINE('',#8469,#1908);
#1599=LINE('',#8475,#1909);
#1600=LINE('',#8483,#1910);
#1601=LINE('',#8488,#1911);
#1602=LINE('',#8497,#1912);
#1603=LINE('',#8503,#1913);
#1604=LINE('',#8511,#1914);
#1605=LINE('',#8513,#1915);
#1606=LINE('',#8515,#1916);
#1607=LINE('',#8516,#1917);
#1608=LINE('',#8519,#1918);
#1609=LINE('',#8521,#1919);
#1610=LINE('',#8522,#1920);
#1611=LINE('',#8525,#1921);
#1612=LINE('',#8527,#1922);
#1613=LINE('',#8528,#1923);
#1614=LINE('',#8531,#1924);
#1615=LINE('',#8533,#1925);
#1616=LINE('',#8534,#1926);
#1617=LINE('',#8537,#1927);
#1618=LINE('',#8539,#1928);
#1619=LINE('',#8540,#1929);
#1620=LINE('',#8542,#1930);
#1621=LINE('',#8543,#1931);
#1622=LINE('',#8555,#1932);
#1623=LINE('',#8559,#1933);
#1624=LINE('',#8563,#1934);
#1625=LINE('',#8570,#1935);
#1626=LINE('',#8572,#1936);
#1627=LINE('',#8587,#1937);
#1628=LINE('',#8593,#1938);
#1629=LINE('',#8597,#1939);
#1630=LINE('',#8603,#1940);
#1631=LINE('',#8608,#1941);
#1632=LINE('',#8623,#1942);
#1633=LINE('',#8632,#1943);
#1634=LINE('',#8636,#1944);
#1635=LINE('',#8640,#1945);
#1636=LINE('',#8643,#1946);
#1637=LINE('',#8779,#1947);
#1638=LINE('',#9032,#1948);
#1639=LINE('',#9074,#1949);
#1640=LINE('',#9079,#1950);
#1641=LINE('',#9088,#1951);
#1642=LINE('',#9093,#1952);
#1643=LINE('',#9104,#1953);
#1644=LINE('',#9106,#1954);
#1645=LINE('',#9108,#1955);
#1646=LINE('',#9109,#1956);
#1647=LINE('',#9114,#1957);
#1648=LINE('',#9115,#1958);
#1649=LINE('',#9118,#1959);
#1650=LINE('',#9120,#1960);
#1651=LINE('',#9121,#1961);
#1652=LINE('',#9123,#1962);
#1653=LINE('',#9137,#1963);
#1654=LINE('',#9140,#1964);
#1655=LINE('',#9145,#1965);
#1656=LINE('',#9153,#1966);
#1657=LINE('',#9159,#1967);
#1658=LINE('',#9164,#1968);
#1659=LINE('',#9181,#1969);
#1660=LINE('',#9232,#1970);
#1661=LINE('',#9236,#1971);
#1662=LINE('',#9238,#1972);
#1663=LINE('',#9240,#1973);
#1664=LINE('',#9241,#1974);
#1665=LINE('',#9244,#1975);
#1666=LINE('',#9246,#1976);
#1667=LINE('',#9247,#1977);
#1668=LINE('',#9250,#1978);
#1669=LINE('',#9252,#1979);
#1670=LINE('',#9253,#1980);
#1671=LINE('',#9263,#1981);
#1672=LINE('',#9265,#1982);
#1673=LINE('',#9267,#1983);
#1674=LINE('',#9268,#1984);
#1675=LINE('',#9272,#1985);
#1676=LINE('',#9274,#1986);
#1677=LINE('',#9276,#1987);
#1678=LINE('',#9277,#1988);
#1679=LINE('',#9284,#1989);
#1680=LINE('',#9288,#1990);
#1681=LINE('',#9292,#1991);
#1682=LINE('',#9296,#1992);
#1683=LINE('',#9302,#1993);
#1684=LINE('',#9305,#1994);
#1685=LINE('',#9306,#1995);
#1686=LINE('',#9309,#1996);
#1687=LINE('',#9311,#1997);
#1688=LINE('',#9312,#1998);
#1689=LINE('',#9316,#1999);
#1690=LINE('',#9319,#2000);
#1691=LINE('',#9320,#2001);
#1692=LINE('',#9323,#2002);
#1693=LINE('',#9325,#2003);
#1694=LINE('',#9326,#2004);
#1695=LINE('',#9336,#2005);
#1696=LINE('',#9339,#2006);
#1697=LINE('',#9347,#2007);
#1698=LINE('',#9353,#2008);
#1699=LINE('',#9361,#2009);
#1700=LINE('',#9378,#2010);
#1701=LINE('',#9429,#2011);
#1702=LINE('',#9434,#2012);
#1703=LINE('',#9440,#2013);
#1704=LINE('',#9449,#2014);
#1705=LINE('',#9456,#2015);
#1706=LINE('',#9462,#2016);
#1707=LINE('',#9472,#2017);
#1708=LINE('',#9479,#2018);
#1709=LINE('',#9482,#2019);
#1710=LINE('',#9491,#2020);
#1711=LINE('',#9497,#2021);
#1712=LINE('',#9506,#2022);
#1713=LINE('',#9512,#2023);
#1714=LINE('',#9520,#2024);
#1715=LINE('',#9522,#2025);
#1716=LINE('',#9524,#2026);
#1717=LINE('',#9525,#2027);
#1718=LINE('',#9529,#2028);
#1719=LINE('',#9535,#2029);
#1720=LINE('',#9536,#2030);
#1721=LINE('',#9537,#2031);
#1722=LINE('',#9543,#2032);
#1723=LINE('',#9546,#2033);
#1724=LINE('',#9549,#2034);
#1725=LINE('',#9550,#2035);
#1726=LINE('',#9554,#2036);
#1727=LINE('',#9556,#2037);
#1728=LINE('',#9557,#2038);
#1729=LINE('',#9560,#2039);
#1730=LINE('',#9565,#2040);
#1731=LINE('',#9566,#2041);
#1732=LINE('',#9567,#2042);
#1733=LINE('',#9572,#2043);
#1734=LINE('',#9579,#2044);
#1735=LINE('',#9581,#2045);
#1736=LINE('',#9583,#2046);
#1737=LINE('',#9584,#2047);
#1738=LINE('',#9587,#2048);
#1739=LINE('',#9589,#2049);
#1740=LINE('',#9590,#2050);
#1741=LINE('',#9593,#2051);
#1742=LINE('',#9595,#2052);
#1743=LINE('',#9596,#2053);
#1744=LINE('',#9599,#2054);
#1745=LINE('',#9601,#2055);
#1746=LINE('',#9602,#2056);
#1747=LINE('',#9605,#2057);
#1748=LINE('',#9607,#2058);
#1749=LINE('',#9608,#2059);
#1750=LINE('',#9610,#2060);
#1751=LINE('',#9611,#2061);
#1752=LINE('',#9619,#2062);
#1753=LINE('',#9623,#2063);
#1754=LINE('',#9627,#2064);
#1755=LINE('',#9633,#2065);
#1756=LINE('',#9635,#2066);
#1757=LINE('',#9637,#2067);
#1758=LINE('',#9638,#2068);
#1759=LINE('',#9641,#2069);
#1760=LINE('',#9643,#2070);
#1761=LINE('',#9644,#2071);
#1762=LINE('',#9647,#2072);
#1763=LINE('',#9649,#2073);
#1764=LINE('',#9650,#2074);
#1765=LINE('',#9653,#2075);
#1766=LINE('',#9655,#2076);
#1767=LINE('',#9656,#2077);
#1768=LINE('',#9659,#2078);
#1769=LINE('',#9661,#2079);
#1770=LINE('',#9662,#2080);
#1771=LINE('',#9664,#2081);
#1772=LINE('',#9665,#2082);
#1773=LINE('',#9677,#2083);
#1774=LINE('',#9681,#2084);
#1775=LINE('',#9685,#2085);
#1776=LINE('',#9692,#2086);
#1777=LINE('',#9694,#2087);
#1778=LINE('',#9709,#2088);
#1779=LINE('',#9715,#2089);
#1780=LINE('',#9719,#2090);
#1781=LINE('',#9725,#2091);
#1782=LINE('',#9730,#2092);
#1783=LINE('',#9745,#2093);
#1784=LINE('',#9754,#2094);
#1785=LINE('',#9758,#2095);
#1786=LINE('',#9762,#2096);
#1787=LINE('',#9765,#2097);
#1788=LINE('',#9918,#2098);
#1789=LINE('',#10214,#2099);
#1790=LINE('',#10256,#2100);
#1791=LINE('',#10261,#2101);
#1792=LINE('',#10270,#2102);
#1793=LINE('',#10275,#2103);
#1794=LINE('',#10288,#2104);
#1795=LINE('',#10292,#2105);
#1796=LINE('',#10296,#2106);
#1797=LINE('',#10303,#2107);
#1798=LINE('',#10307,#2108);
#1799=LINE('',#10311,#2109);
#1800=LINE('',#10316,#2110);
#1801=LINE('',#10318,#2111);
#1802=LINE('',#10320,#2112);
#1803=LINE('',#10321,#2113);
#1804=LINE('',#10324,#2114);
#1805=LINE('',#10326,#2115);
#1806=LINE('',#10327,#2116);
#1807=LINE('',#10330,#2117);
#1808=LINE('',#10332,#2118);
#1809=LINE('',#10333,#2119);
#1810=LINE('',#10336,#2120);
#1811=LINE('',#10338,#2121);
#1812=LINE('',#10339,#2122);
#1813=LINE('',#10342,#2123);
#1814=LINE('',#10344,#2124);
#1815=LINE('',#10345,#2125);
#1816=LINE('',#10347,#2126);
#1817=LINE('',#10348,#2127);
#1818=LINE('',#10396,#2128);
#1819=LINE('',#10403,#2129);
#1820=LINE('',#10409,#2130);
#1821=LINE('',#10418,#2131);
#1822=LINE('',#10424,#2132);
#1823=VECTOR('',#6429,0.25);
#1824=VECTOR('',#6436,0.25);
#1825=VECTOR('',#6443,0.25);
#1826=VECTOR('',#6450,0.25);
#1827=VECTOR('',#6455,1.);
#1828=VECTOR('',#6456,1.);
#1829=VECTOR('',#6457,1.);
#1830=VECTOR('',#6458,1.);
#1831=VECTOR('',#6461,1.);
#1832=VECTOR('',#6462,1.);
#1833=VECTOR('',#6463,1.);
#1834=VECTOR('',#6466,1.);
#1835=VECTOR('',#6467,1.);
#1836=VECTOR('',#6468,1.);
#1837=VECTOR('',#6471,1.);
#1838=VECTOR('',#6472,1.);
#1839=VECTOR('',#6481,1.);
#1840=VECTOR('',#6482,1.);
#1841=VECTOR('',#6483,1.);
#1842=VECTOR('',#6484,1.);
#1843=VECTOR('',#6487,1.);
#1844=VECTOR('',#6488,1.);
#1845=VECTOR('',#6489,1.);
#1846=VECTOR('',#6492,1.);
#1847=VECTOR('',#6493,1.);
#1848=VECTOR('',#6494,1.);
#1849=VECTOR('',#6497,1.);
#1850=VECTOR('',#6498,1.);
#1851=VECTOR('',#6507,1.);
#1852=VECTOR('',#6508,1.);
#1853=VECTOR('',#6509,1.);
#1854=VECTOR('',#6510,1.);
#1855=VECTOR('',#6513,1.);
#1856=VECTOR('',#6514,1.);
#1857=VECTOR('',#6515,1.);
#1858=VECTOR('',#6518,1.);
#1859=VECTOR('',#6519,1.);
#1860=VECTOR('',#6520,1.);
#1861=VECTOR('',#6523,1.);
#1862=VECTOR('',#6524,1.);
#1863=VECTOR('',#6535,0.165);
#1864=VECTOR('',#6542,0.165);
#1865=VECTOR('',#6549,0.165);
#1866=VECTOR('',#6556,0.165);
#1867=VECTOR('',#6563,0.33);
#1868=VECTOR('',#6570,0.33);
#1869=VECTOR('',#6577,0.33);
#1870=VECTOR('',#6584,0.33);
#1871=VECTOR('',#6591,1.6);
#1872=VECTOR('',#6596,1.);
#1873=VECTOR('',#6597,1.);
#1874=VECTOR('',#6598,1.);
#1875=VECTOR('',#6599,1.);
#1876=VECTOR('',#6602,1.);
#1877=VECTOR('',#6603,1.);
#1878=VECTOR('',#6604,1.);
#1879=VECTOR('',#6605,1.);
#1880=VECTOR('',#6608,1.);
#1881=VECTOR('',#6609,1.);
#1882=VECTOR('',#6610,1.);
#1883=VECTOR('',#6613,1.);
#1884=VECTOR('',#6614,1.);
#1885=VECTOR('',#6615,1.);
#1886=VECTOR('',#6618,1.);
#1887=VECTOR('',#6619,1.);
#1888=VECTOR('',#6620,1.);
#1889=VECTOR('',#6621,1.);
#1890=VECTOR('',#6624,1.);
#1891=VECTOR('',#6625,1.);
#1892=VECTOR('',#6628,1.);
#1893=VECTOR('',#6629,1.);
#1894=VECTOR('',#6630,1.);
#1895=VECTOR('',#6633,1.);
#1896=VECTOR('',#6644,1.2);
#1897=VECTOR('',#6651,1.59);
#1898=VECTOR('',#6664,0.225);
#1899=VECTOR('',#6671,0.225);
#1900=VECTOR('',#6678,0.225);
#1901=VECTOR('',#6685,0.225);
#1902=VECTOR('',#6692,1.59);
#1903=VECTOR('',#6701,1.2);
#1904=VECTOR('',#6708,2.4);
#1905=VECTOR('',#6721,0.225);
#1906=VECTOR('',#6728,0.225);
#1907=VECTOR('',#6735,0.225);
#1908=VECTOR('',#6742,0.225);
#1909=VECTOR('',#6749,1.59);
#1910=VECTOR('',#6760,1.2);
#1911=VECTOR('',#6765,2.4);
#1912=VECTOR('',#6778,0.32);
#1913=VECTOR('',#6785,0.6);
#1914=VECTOR('',#6796,1.);
#1915=VECTOR('',#6797,1.);
#1916=VECTOR('',#6798,1.);
#1917=VECTOR('',#6799,1.);
#1918=VECTOR('',#6802,1.);
#1919=VECTOR('',#6803,1.);
#1920=VECTOR('',#6804,1.);
#1921=VECTOR('',#6807,1.);
#1922=VECTOR('',#6808,1.);
#1923=VECTOR('',#6809,1.);
#1924=VECTOR('',#6812,1.);
#1925=VECTOR('',#6813,1.);
#1926=VECTOR('',#6814,1.);
#1927=VECTOR('',#6817,1.);
#1928=VECTOR('',#6818,1.);
#1929=VECTOR('',#6819,1.);
#1930=VECTOR('',#6822,1.);
#1931=VECTOR('',#6823,1.);
#1932=VECTOR('',#6840,0.475);
#1933=VECTOR('',#6845,0.5);
#1934=VECTOR('',#6850,0.485);
#1935=VECTOR('',#6859,0.31);
#1936=VECTOR('',#6862,0.3);
#1937=VECTOR('',#6881,1.070235);
#1938=VECTOR('',#6888,0.6);
#1939=VECTOR('',#6893,0.63);
#1940=VECTOR('',#6902,1.070235);
#1941=VECTOR('',#6909,0.63);
#1942=VECTOR('',#6928,1.129765);
#1943=VECTOR('',#6939,1.57);
#1944=VECTOR('',#6944,1.6);
#1945=VECTOR('',#6949,1.57);
#1946=VECTOR('',#6954,1.129765);
#1947=VECTOR('',#7001,1.123812);
#1948=VECTOR('',#7070,1.076188);
#1949=VECTOR('',#7099,1.119765);
#1950=VECTOR('',#7106,1.085235);
#1951=VECTOR('',#7117,1.119765);
#1952=VECTOR('',#7124,1.085235);
#1953=VECTOR('',#7141,1.);
#1954=VECTOR('',#7142,1.);
#1955=VECTOR('',#7143,1.);
#1956=VECTOR('',#7144,1.);
#1957=VECTOR('',#7149,1.);
#1958=VECTOR('',#7150,1.);
#1959=VECTOR('',#7153,1.);
#1960=VECTOR('',#7154,1.);
#1961=VECTOR('',#7155,1.);
#1962=VECTOR('',#7158,1.);
#1963=VECTOR('',#7177,0.8);
#1964=VECTOR('',#7180,0.6);
#1965=VECTOR('',#7187,0.6);
#1966=VECTOR('',#7198,0.165);
#1967=VECTOR('',#7205,0.165);
#1968=VECTOR('',#7210,1.);
#1969=VECTOR('',#7217,0.21);
#1970=VECTOR('',#7222,1.);
#1971=VECTOR('',#7225,1.);
#1972=VECTOR('',#7226,1.);
#1973=VECTOR('',#7227,1.);
#1974=VECTOR('',#7228,1.);
#1975=VECTOR('',#7231,1.);
#1976=VECTOR('',#7232,1.);
#1977=VECTOR('',#7233,1.);
#1978=VECTOR('',#7236,1.);
#1979=VECTOR('',#7237,1.);
#1980=VECTOR('',#7238,1.);
#1981=VECTOR('',#7251,1.);
#1982=VECTOR('',#7252,1.);
#1983=VECTOR('',#7253,1.);
#1984=VECTOR('',#7254,1.);
#1985=VECTOR('',#7257,1.);
#1986=VECTOR('',#7258,1.);
#1987=VECTOR('',#7259,1.);
#1988=VECTOR('',#7260,1.);
#1989=VECTOR('',#7267,1.);
#1990=VECTOR('',#7270,1.);
#1991=VECTOR('',#7273,1.);
#1992=VECTOR('',#7276,1.);
#1993=VECTOR('',#7285,1.);
#1994=VECTOR('',#7288,1.);
#1995=VECTOR('',#7289,1.);
#1996=VECTOR('',#7292,1.);
#1997=VECTOR('',#7293,1.);
#1998=VECTOR('',#7294,1.);
#1999=VECTOR('',#7299,1.);
#2000=VECTOR('',#7302,1.);
#2001=VECTOR('',#7303,1.);
#2002=VECTOR('',#7306,1.);
#2003=VECTOR('',#7307,1.);
#2004=VECTOR('',#7308,1.);
#2005=VECTOR('',#7325,8.);
#2006=VECTOR('',#7328,1.5);
#2007=VECTOR('',#7339,0.605);
#2008=VECTOR('',#7346,0.8);
#2009=VECTOR('',#7357,1.);
#2010=VECTOR('',#7364,0.21);
#2011=VECTOR('',#7369,1.);
#2012=VECTOR('',#7374,0.605);
#2013=VECTOR('',#7381,1.1);
#2014=VECTOR('',#7394,0.165);
#2015=VECTOR('',#7403,0.225);
#2016=VECTOR('',#7410,0.225);
#2017=VECTOR('',#7423,1.7);
#2018=VECTOR('',#7432,0.7);
#2019=VECTOR('',#7435,0.5);
#2020=VECTOR('',#7448,0.505);
#2021=VECTOR('',#7455,0.7);
#2022=VECTOR('',#7468,0.225);
#2023=VECTOR('',#7475,0.9);
#2024=VECTOR('',#7486,1.);
#2025=VECTOR('',#7487,1.);
#2026=VECTOR('',#7488,1.);
#2027=VECTOR('',#7489,1.);
#2028=VECTOR('',#7492,1.);
#2029=VECTOR('',#7499,1.);
#2030=VECTOR('',#7500,1.);
#2031=VECTOR('',#7501,1.);
#2032=VECTOR('',#7510,1.);
#2033=VECTOR('',#7513,1.);
#2034=VECTOR('',#7516,1.);
#2035=VECTOR('',#7517,1.);
#2036=VECTOR('',#7522,1.);
#2037=VECTOR('',#7523,1.);
#2038=VECTOR('',#7524,1.);
#2039=VECTOR('',#7527,1.);
#2040=VECTOR('',#7532,1.);
#2041=VECTOR('',#7533,1.);
#2042=VECTOR('',#7534,1.);
#2043=VECTOR('',#7543,1.);
#2044=VECTOR('',#7552,1.);
#2045=VECTOR('',#7553,1.);
#2046=VECTOR('',#7554,1.);
#2047=VECTOR('',#7555,1.);
#2048=VECTOR('',#7558,1.);
#2049=VECTOR('',#7559,1.);
#2050=VECTOR('',#7560,1.);
#2051=VECTOR('',#7563,1.);
#2052=VECTOR('',#7564,1.);
#2053=VECTOR('',#7565,1.);
#2054=VECTOR('',#7568,1.);
#2055=VECTOR('',#7569,1.);
#2056=VECTOR('',#7570,1.);
#2057=VECTOR('',#7573,1.);
#2058=VECTOR('',#7574,1.);
#2059=VECTOR('',#7575,1.);
#2060=VECTOR('',#7578,1.);
#2061=VECTOR('',#7579,1.);
#2062=VECTOR('',#7590,0.235);
#2063=VECTOR('',#7595,0.25);
#2064=VECTOR('',#7600,0.2125);
#2065=VECTOR('',#7607,1.);
#2066=VECTOR('',#7608,1.);
#2067=VECTOR('',#7609,1.);
#2068=VECTOR('',#7610,1.);
#2069=VECTOR('',#7613,1.);
#2070=VECTOR('',#7614,1.);
#2071=VECTOR('',#7615,1.);
#2072=VECTOR('',#7618,1.);
#2073=VECTOR('',#7619,1.);
#2074=VECTOR('',#7620,1.);
#2075=VECTOR('',#7623,1.);
#2076=VECTOR('',#7624,1.);
#2077=VECTOR('',#7625,1.);
#2078=VECTOR('',#7628,1.);
#2079=VECTOR('',#7629,1.);
#2080=VECTOR('',#7630,1.);
#2081=VECTOR('',#7633,1.);
#2082=VECTOR('',#7634,1.);
#2083=VECTOR('',#7651,0.325);
#2084=VECTOR('',#7656,0.35);
#2085=VECTOR('',#7661,0.335);
#2086=VECTOR('',#7670,0.21);
#2087=VECTOR('',#7673,0.2);
#2088=VECTOR('',#7692,0.976185);
#2089=VECTOR('',#7699,0.5);
#2090=VECTOR('',#7704,0.53);
#2091=VECTOR('',#7713,0.976185);
#2092=VECTOR('',#7720,0.53);
#2093=VECTOR('',#7739,1.023815);
#2094=VECTOR('',#7750,1.47);
#2095=VECTOR('',#7755,1.5);
#2096=VECTOR('',#7760,1.47);
#2097=VECTOR('',#7765,1.023815);
#2098=VECTOR('',#7816,1.019052);
#2099=VECTOR('',#7893,0.980948);
#2100=VECTOR('',#7922,1.013815);
#2101=VECTOR('',#7929,0.991185);
#2102=VECTOR('',#7940,1.013815);
#2103=VECTOR('',#7947,0.991185);
#2104=VECTOR('',#7968,0.325);
#2105=VECTOR('',#7973,0.35);
#2106=VECTOR('',#7978,0.335);
#2107=VECTOR('',#7987,0.21);
#2108=VECTOR('',#7992,0.2);
#2109=VECTOR('',#7997,0.18);
#2110=VECTOR('',#8002,1.);
#2111=VECTOR('',#8003,1.);
#2112=VECTOR('',#8004,1.);
#2113=VECTOR('',#8005,1.);
#2114=VECTOR('',#8008,1.);
#2115=VECTOR('',#8009,1.);
#2116=VECTOR('',#8010,1.);
#2117=VECTOR('',#8013,1.);
#2118=VECTOR('',#8014,1.);
#2119=VECTOR('',#8015,1.);
#2120=VECTOR('',#8018,1.);
#2121=VECTOR('',#8019,1.);
#2122=VECTOR('',#8020,1.);
#2123=VECTOR('',#8023,1.);
#2124=VECTOR('',#8024,1.);
#2125=VECTOR('',#8025,1.);
#2126=VECTOR('',#8028,1.);
#2127=VECTOR('',#8029,1.);
#2128=VECTOR('',#8120,1.5);
#2129=VECTOR('',#8129,0.91);
#2130=VECTOR('',#8136,1.8);
#2131=VECTOR('',#8149,0.91);
#2132=VECTOR('',#8156,1.8);
#2133=CIRCLE('',#5701,0.25);
#2134=CIRCLE('',#5702,0.25);
#2135=CIRCLE('',#5704,0.25);
#2136=CIRCLE('',#5705,0.25);
#2137=CIRCLE('',#5707,0.25);
#2138=CIRCLE('',#5708,0.25);
#2139=CIRCLE('',#5710,0.25);
#2140=CIRCLE('',#5711,0.25);
#2141=CIRCLE('',#5734,0.165);
#2142=CIRCLE('',#5735,0.165);
#2143=CIRCLE('',#5737,0.165);
#2144=CIRCLE('',#5738,0.165);
#2145=CIRCLE('',#5740,0.165);
#2146=CIRCLE('',#5741,0.165);
#2147=CIRCLE('',#5743,0.165);
#2148=CIRCLE('',#5744,0.165);
#2149=CIRCLE('',#5746,0.33);
#2150=CIRCLE('',#5747,0.33);
#2151=CIRCLE('',#5749,0.33);
#2152=CIRCLE('',#5750,0.33);
#2153=CIRCLE('',#5752,0.33);
#2154=CIRCLE('',#5753,0.33);
#2155=CIRCLE('',#5755,0.33);
#2156=CIRCLE('',#5756,0.33);
#2157=CIRCLE('',#5758,1.6);
#2158=CIRCLE('',#5759,1.6);
#2159=CIRCLE('',#5772,1.2);
#2160=CIRCLE('',#5773,1.2);
#2161=CIRCLE('',#5775,1.59);
#2162=CIRCLE('',#5776,1.59);
#2163=CIRCLE('',#5781,0.225);
#2164=CIRCLE('',#5782,0.225);
#2165=CIRCLE('',#5784,0.225);
#2166=CIRCLE('',#5785,0.225);
#2167=CIRCLE('',#5787,0.225);
#2168=CIRCLE('',#5788,0.225);
#2169=CIRCLE('',#5790,0.225);
#2170=CIRCLE('',#5791,0.225);
#2171=CIRCLE('',#5793,1.59);
#2172=CIRCLE('',#5794,1.59);
#2173=CIRCLE('',#5796,1.2);
#2174=CIRCLE('',#5798,1.2);
#2175=CIRCLE('',#5800,2.4);
#2176=CIRCLE('',#5801,2.4);
#2177=CIRCLE('',#5806,0.225);
#2178=CIRCLE('',#5807,0.225);
#2179=CIRCLE('',#5809,0.225);
#2180=CIRCLE('',#5810,0.225);
#2181=CIRCLE('',#5812,0.225);
#2182=CIRCLE('',#5813,0.225);
#2183=CIRCLE('',#5815,0.225);
#2184=CIRCLE('',#5816,0.225);
#2185=CIRCLE('',#5818,1.59);
#2186=CIRCLE('',#5819,1.59);
#2187=CIRCLE('',#5821,1.2);
#2188=CIRCLE('',#5823,1.2);
#2189=CIRCLE('',#5825,2.4);
#2190=CIRCLE('',#5826,2.4);
#2191=CIRCLE('',#5831,0.32);
#2192=CIRCLE('',#5832,0.32);
#2193=CIRCLE('',#5834,0.6);
#2194=CIRCLE('',#5835,0.6);
#2195=CIRCLE('',#5848,0.2942);
#2196=CIRCLE('',#5850,0.45);
#2197=CIRCLE('',#5852,0.5);
#2198=CIRCLE('',#5854,0.5);
#2199=CIRCLE('',#5856,0.47);
#2200=CIRCLE('',#5858,0.32);
#2201=CIRCLE('',#5860,0.2942);
#2202=CIRCLE('',#5865,1.070235);
#2203=CIRCLE('',#5866,1.070235);
#2204=CIRCLE('',#5867,0.309556);
#2205=CIRCLE('',#5868,1.070235);
#2206=CIRCLE('',#5869,1.070235);
#2207=CIRCLE('',#5871,1.070235);
#2208=CIRCLE('',#5873,0.6);
#2209=CIRCLE('',#5874,0.6);
#2210=CIRCLE('',#5876,0.66);
#2211=CIRCLE('',#5879,1.070235);
#2212=CIRCLE('',#5881,0.66);
#2213=CIRCLE('',#5885,1.129765);
#2214=CIRCLE('',#5886,1.129765);
#2215=CIRCLE('',#5887,0.309556);
#2216=CIRCLE('',#5888,1.129765);
#2217=CIRCLE('',#5889,1.129765);
#2218=CIRCLE('',#5891,1.129765);
#2219=CIRCLE('',#5893,1.54);
#2220=CIRCLE('',#5894,1.129765);
#2221=CIRCLE('',#5896,1.6);
#2222=CIRCLE('',#5898,1.6);
#2223=CIRCLE('',#5900,1.54);
#2224=CIRCLE('',#5905,0.29765);
#2225=CIRCLE('',#5907,0.29765);
#2226=CIRCLE('',#5909,0.29765);
#2227=CIRCLE('',#5911,0.29765);
#2228=CIRCLE('',#5913,0.29765);
#2229=CIRCLE('',#5915,0.29765);
#2230=CIRCLE('',#5917,0.29765);
#2231=CIRCLE('',#5920,0.303778037777585);
#2232=CIRCLE('',#5921,0.303778037777585);
#2233=CIRCLE('',#5923,1.123812);
#2234=CIRCLE('',#5924,1.123812);
#2235=CIRCLE('',#5925,1.123812);
#2236=CIRCLE('',#5926,1.123812);
#2237=CIRCLE('',#5927,1.123812);
#2238=CIRCLE('',#5928,1.123812);
#2239=CIRCLE('',#5929,1.123812);
#2240=CIRCLE('',#5930,1.123812);
#2241=CIRCLE('',#5931,1.123812);
#2242=CIRCLE('',#5933,1.076188);
#2243=CIRCLE('',#5934,0.303778037777585);
#2244=CIRCLE('',#5936,0.303778037777585);
#2245=CIRCLE('',#5938,1.076188);
#2246=CIRCLE('',#5939,0.303778037777585);
#2247=CIRCLE('',#5941,0.303778037777585);
#2248=CIRCLE('',#5943,1.076188);
#2249=CIRCLE('',#5944,1.076188);
#2250=CIRCLE('',#5945,0.303778037777585);
#2251=CIRCLE('',#5947,0.303778037777585);
#2252=CIRCLE('',#5949,1.076188);
#2253=CIRCLE('',#5950,0.303778037777585);
#2254=CIRCLE('',#5952,0.303778037777585);
#2255=CIRCLE('',#5954,1.076188);
#2256=CIRCLE('',#5955,0.303778037777585);
#2257=CIRCLE('',#5957,0.303778037777585);
#2258=CIRCLE('',#5959,1.076188);
#2259=CIRCLE('',#5960,1.076188);
#2260=CIRCLE('',#5961,1.076188);
#2261=CIRCLE('',#5963,0.303778037777585);
#2262=CIRCLE('',#5965,0.303778037777585);
#2263=CIRCLE('',#5970,1.119765);
#2264=CIRCLE('',#5971,1.085235);
#2265=CIRCLE('',#5973,1.119765);
#2266=CIRCLE('',#5975,1.085235);
#2267=CIRCLE('',#5978,1.119765);
#2268=CIRCLE('',#5979,1.085235);
#2269=CIRCLE('',#5981,1.119765);
#2270=CIRCLE('',#5983,1.085235);
#2271=CIRCLE('',#5994,0.6);
#2272=CIRCLE('',#5998,0.6);
#2273=CIRCLE('',#6000,0.8);
#2274=CIRCLE('',#6001,0.6);
#2275=CIRCLE('',#6003,0.8);
#2276=CIRCLE('',#6004,0.6);
#2277=CIRCLE('',#6007,0.6);
#2278=CIRCLE('',#6009,0.6);
#2279=CIRCLE('',#6014,0.165);
#2280=CIRCLE('',#6015,0.165);
#2281=CIRCLE('',#6017,0.165);
#2282=CIRCLE('',#6018,0.165);
#2283=CIRCLE('',#6020,0.21);
#2284=CIRCLE('',#6022,0.21);
#2285=CIRCLE('',#6023,0.21);
#2286=CIRCLE('',#6029,1.5);
#2287=CIRCLE('',#6030,0.6);
#2288=CIRCLE('',#6032,0.6);
#2289=CIRCLE('',#6036,8.);
#2290=CIRCLE('',#6037,7.25);
#2291=CIRCLE('',#6038,1.5);
#2292=CIRCLE('',#6039,7.25);
#2293=CIRCLE('',#6040,1.5);
#2294=CIRCLE('',#6041,7.25);
#2295=CIRCLE('',#6042,1.5);
#2296=CIRCLE('',#6044,7.25);
#2297=CIRCLE('',#6048,7.25);
#2298=CIRCLE('',#6052,8.);
#2299=CIRCLE('',#6053,7.25);
#2300=CIRCLE('',#6054,1.5);
#2301=CIRCLE('',#6055,1.5);
#2302=CIRCLE('',#6056,1.5);
#2303=CIRCLE('',#6060,1.5);
#2304=CIRCLE('',#6064,0.605);
#2305=CIRCLE('',#6065,0.605);
#2306=CIRCLE('',#6067,0.8);
#2307=CIRCLE('',#6068,0.8);
#2308=CIRCLE('',#6073,0.21);
#2309=CIRCLE('',#6075,0.21);
#2310=CIRCLE('',#6076,0.21);
#2311=CIRCLE('',#6079,0.605);
#2312=CIRCLE('',#6080,0.605);
#2313=CIRCLE('',#6082,1.1);
#2314=CIRCLE('',#6083,1.1);
#2315=CIRCLE('',#6088,0.165);
#2316=CIRCLE('',#6089,0.165);
#2317=CIRCLE('',#6092,0.225);
#2318=CIRCLE('',#6093,0.225);
#2319=CIRCLE('',#6095,0.225);
#2320=CIRCLE('',#6096,0.225);
#2321=CIRCLE('',#6098,1.7);
#2322=CIRCLE('',#6099,0.7);
#2323=CIRCLE('',#6101,1.7);
#2324=CIRCLE('',#6103,0.7);
#2325=CIRCLE('',#6104,0.5);
#2326=CIRCLE('',#6107,0.5);
#2327=CIRCLE('',#6112,0.505);
#2328=CIRCLE('',#6113,0.505);
#2329=CIRCLE('',#6115,0.7);
#2330=CIRCLE('',#6116,0.7);
#2331=CIRCLE('',#6121,0.225);
#2332=CIRCLE('',#6122,0.225);
#2333=CIRCLE('',#6124,0.9);
#2334=CIRCLE('',#6125,0.9);
#2335=CIRCLE('',#6131,0.16);
#2336=CIRCLE('',#6132,0.2);
#2337=CIRCLE('',#6135,0.16);
#2338=CIRCLE('',#6136,0.2);
#2339=CIRCLE('',#6138,0.2);
#2340=CIRCLE('',#6143,0.16);
#2341=CIRCLE('',#6146,0.2);
#2342=CIRCLE('',#6147,0.16);
#2343=CIRCLE('',#6160,0.22);
#2344=CIRCLE('',#6162,0.24505);
#2345=CIRCLE('',#6164,0.24505);
#2346=CIRCLE('',#6166,0.175);
#2347=CIRCLE('',#6178,0.1954);
#2348=CIRCLE('',#6180,0.3);
#2349=CIRCLE('',#6182,0.35);
#2350=CIRCLE('',#6184,0.35);
#2351=CIRCLE('',#6186,0.32);
#2352=CIRCLE('',#6188,0.22);
#2353=CIRCLE('',#6190,0.1954);
#2354=CIRCLE('',#6195,0.976185);
#2355=CIRCLE('',#6196,0.976185);
#2356=CIRCLE('',#6197,0.247676);
#2357=CIRCLE('',#6198,0.976185);
#2358=CIRCLE('',#6199,0.976185);
#2359=CIRCLE('',#6201,0.976185);
#2360=CIRCLE('',#6203,0.5);
#2361=CIRCLE('',#6204,0.5);
#2362=CIRCLE('',#6206,0.56);
#2363=CIRCLE('',#6209,0.976185);
#2364=CIRCLE('',#6211,0.56);
#2365=CIRCLE('',#6215,1.023815);
#2366=CIRCLE('',#6216,1.023815);
#2367=CIRCLE('',#6217,0.247676);
#2368=CIRCLE('',#6218,1.023815);
#2369=CIRCLE('',#6219,1.023815);
#2370=CIRCLE('',#6221,1.023815);
#2371=CIRCLE('',#6223,1.44);
#2372=CIRCLE('',#6224,1.023815);
#2373=CIRCLE('',#6226,1.5);
#2374=CIRCLE('',#6228,1.5);
#2375=CIRCLE('',#6230,1.44);
#2376=CIRCLE('',#6235,0.23815);
#2377=CIRCLE('',#6237,0.23815);
#2378=CIRCLE('',#6239,0.23815);
#2379=CIRCLE('',#6241,0.23815);
#2380=CIRCLE('',#6243,0.23815);
#2381=CIRCLE('',#6245,0.23815);
#2382=CIRCLE('',#6247,0.23815);
#2383=CIRCLE('',#6249,0.23815);
#2384=CIRCLE('',#6252,0.243053047864041);
#2385=CIRCLE('',#6253,0.243053047864041);
#2386=CIRCLE('',#6255,1.019052);
#2387=CIRCLE('',#6256,1.019052);
#2388=CIRCLE('',#6257,1.019052);
#2389=CIRCLE('',#6258,1.019052);
#2390=CIRCLE('',#6259,1.019052);
#2391=CIRCLE('',#6260,1.019052);
#2392=CIRCLE('',#6261,1.019052);
#2393=CIRCLE('',#6262,1.019052);
#2394=CIRCLE('',#6263,1.019052);
#2395=CIRCLE('',#6265,0.980948);
#2396=CIRCLE('',#6266,0.243053047864041);
#2397=CIRCLE('',#6268,0.243053047864041);
#2398=CIRCLE('',#6270,0.980948);
#2399=CIRCLE('',#6271,0.243053047864041);
#2400=CIRCLE('',#6273,0.243053047864041);
#2401=CIRCLE('',#6275,0.980948);
#2402=CIRCLE('',#6276,0.243053047864041);
#2403=CIRCLE('',#6278,0.243053047864041);
#2404=CIRCLE('',#6280,0.980948);
#2405=CIRCLE('',#6281,0.243053047864041);
#2406=CIRCLE('',#6283,0.243053047864041);
#2407=CIRCLE('',#6285,0.980948);
#2408=CIRCLE('',#6286,0.243053047864041);
#2409=CIRCLE('',#6288,0.243053047864041);
#2410=CIRCLE('',#6290,0.980948);
#2411=CIRCLE('',#6291,0.243053047864041);
#2412=CIRCLE('',#6293,0.243053047864041);
#2413=CIRCLE('',#6295,0.980948);
#2414=CIRCLE('',#6296,0.980948);
#2415=CIRCLE('',#6297,0.980948);
#2416=CIRCLE('',#6299,0.243053047864041);
#2417=CIRCLE('',#6301,0.243053047864041);
#2418=CIRCLE('',#6306,1.013815);
#2419=CIRCLE('',#6307,0.991185);
#2420=CIRCLE('',#6309,1.013815);
#2421=CIRCLE('',#6311,0.991185);
#2422=CIRCLE('',#6314,1.013815);
#2423=CIRCLE('',#6315,0.991185);
#2424=CIRCLE('',#6317,1.013815);
#2425=CIRCLE('',#6319,0.991185);
#2426=CIRCLE('',#6328,0.3);
#2427=CIRCLE('',#6330,0.35);
#2428=CIRCLE('',#6332,0.35);
#2429=CIRCLE('',#6334,0.32);
#2430=CIRCLE('',#6336,0.22);
#2431=CIRCLE('',#6338,0.1954);
#2432=CIRCLE('',#6340,0.1954);
#2433=CIRCLE('',#6342,0.16);
#2434=CIRCLE('',#6394,1.5);
#2435=CIRCLE('',#6395,1.5);
#2436=CIRCLE('',#6397,0.91);
#2437=CIRCLE('',#6399,0.91);
#2438=CIRCLE('',#6401,1.8);
#2439=CIRCLE('',#6402,1.8);
#2440=CIRCLE('',#6407,0.91);
#2441=CIRCLE('',#6408,0.91);
#2442=CIRCLE('',#6410,1.8);
#2443=CIRCLE('',#6411,1.8);
#2444=VERTEX_POINT('',#8177);
#2445=VERTEX_POINT('',#8179);
#2446=VERTEX_POINT('',#8183);
#2447=VERTEX_POINT('',#8185);
#2448=VERTEX_POINT('',#8189);
#2449=VERTEX_POINT('',#8191);
#2450=VERTEX_POINT('',#8195);
#2451=VERTEX_POINT('',#8197);
#2452=VERTEX_POINT('',#8201);
#2453=VERTEX_POINT('',#8202);
#2454=VERTEX_POINT('',#8204);
#2455=VERTEX_POINT('',#8206);
#2456=VERTEX_POINT('',#8210);
#2457=VERTEX_POINT('',#8212);
#2458=VERTEX_POINT('',#8216);
#2459=VERTEX_POINT('',#8218);
#2460=VERTEX_POINT('',#8228);
#2461=VERTEX_POINT('',#8229);
#2462=VERTEX_POINT('',#8231);
#2463=VERTEX_POINT('',#8233);
#2464=VERTEX_POINT('',#8237);
#2465=VERTEX_POINT('',#8239);
#2466=VERTEX_POINT('',#8243);
#2467=VERTEX_POINT('',#8245);
#2468=VERTEX_POINT('',#8255);
#2469=VERTEX_POINT('',#8256);
#2470=VERTEX_POINT('',#8258);
#2471=VERTEX_POINT('',#8260);
#2472=VERTEX_POINT('',#8264);
#2473=VERTEX_POINT('',#8266);
#2474=VERTEX_POINT('',#8270);
#2475=VERTEX_POINT('',#8272);
#2476=VERTEX_POINT('',#8282);
#2477=VERTEX_POINT('',#8284);
#2478=VERTEX_POINT('',#8288);
#2479=VERTEX_POINT('',#8290);
#2480=VERTEX_POINT('',#8294);
#2481=VERTEX_POINT('',#8296);
#2482=VERTEX_POINT('',#8300);
#2483=VERTEX_POINT('',#8302);
#2484=VERTEX_POINT('',#8306);
#2485=VERTEX_POINT('',#8308);
#2486=VERTEX_POINT('',#8312);
#2487=VERTEX_POINT('',#8314);
#2488=VERTEX_POINT('',#8318);
#2489=VERTEX_POINT('',#8320);
#2490=VERTEX_POINT('',#8324);
#2491=VERTEX_POINT('',#8326);
#2492=VERTEX_POINT('',#8330);
#2493=VERTEX_POINT('',#8332);
#2494=VERTEX_POINT('',#8336);
#2495=VERTEX_POINT('',#8337);
#2496=VERTEX_POINT('',#8339);
#2497=VERTEX_POINT('',#8341);
#2498=VERTEX_POINT('',#8345);
#2499=VERTEX_POINT('',#8346);
#2500=VERTEX_POINT('',#8348);
#2501=VERTEX_POINT('',#8350);
#2502=VERTEX_POINT('',#8354);
#2503=VERTEX_POINT('',#8356);
#2504=VERTEX_POINT('',#8360);
#2505=VERTEX_POINT('',#8362);
#2506=VERTEX_POINT('',#8366);
#2507=VERTEX_POINT('',#8368);
#2508=VERTEX_POINT('',#8373);
#2509=VERTEX_POINT('',#8377);
#2510=VERTEX_POINT('',#8387);
#2511=VERTEX_POINT('',#8389);
#2512=VERTEX_POINT('',#8393);
#2513=VERTEX_POINT('',#8395);
#2514=VERTEX_POINT('',#8402);
#2515=VERTEX_POINT('',#8404);
#2516=VERTEX_POINT('',#8408);
#2517=VERTEX_POINT('',#8410);
#2518=VERTEX_POINT('',#8414);
#2519=VERTEX_POINT('',#8416);
#2520=VERTEX_POINT('',#8420);
#2521=VERTEX_POINT('',#8422);
#2522=VERTEX_POINT('',#8426);
#2523=VERTEX_POINT('',#8428);
#2524=VERTEX_POINT('',#8432);
#2525=VERTEX_POINT('',#8435);
#2526=VERTEX_POINT('',#8439);
#2527=VERTEX_POINT('',#8441);
#2528=VERTEX_POINT('',#8448);
#2529=VERTEX_POINT('',#8450);
#2530=VERTEX_POINT('',#8454);
#2531=VERTEX_POINT('',#8456);
#2532=VERTEX_POINT('',#8460);
#2533=VERTEX_POINT('',#8462);
#2534=VERTEX_POINT('',#8466);
#2535=VERTEX_POINT('',#8468);
#2536=VERTEX_POINT('',#8472);
#2537=VERTEX_POINT('',#8474);
#2538=VERTEX_POINT('',#8478);
#2539=VERTEX_POINT('',#8481);
#2540=VERTEX_POINT('',#8485);
#2541=VERTEX_POINT('',#8487);
#2542=VERTEX_POINT('',#8494);
#2543=VERTEX_POINT('',#8496);
#2544=VERTEX_POINT('',#8500);
#2545=VERTEX_POINT('',#8502);
#2546=VERTEX_POINT('',#8509);
#2547=VERTEX_POINT('',#8510);
#2548=VERTEX_POINT('',#8512);
#2549=VERTEX_POINT('',#8514);
#2550=VERTEX_POINT('',#8518);
#2551=VERTEX_POINT('',#8520);
#2552=VERTEX_POINT('',#8524);
#2553=VERTEX_POINT('',#8526);
#2554=VERTEX_POINT('',#8530);
#2555=VERTEX_POINT('',#8532);
#2556=VERTEX_POINT('',#8536);
#2557=VERTEX_POINT('',#8538);
#2558=VERTEX_POINT('',#8547);
#2559=VERTEX_POINT('',#8550);
#2560=VERTEX_POINT('',#8553);
#2561=VERTEX_POINT('',#8557);
#2562=VERTEX_POINT('',#8561);
#2563=VERTEX_POINT('',#8565);
#2564=VERTEX_POINT('',#8568);
#2565=VERTEX_POINT('',#8576);
#2566=VERTEX_POINT('',#8577);
#2567=VERTEX_POINT('',#8580);
#2568=VERTEX_POINT('',#8582);
#2569=VERTEX_POINT('',#8586);
#2570=VERTEX_POINT('',#8590);
#2571=VERTEX_POINT('',#8592);
#2572=VERTEX_POINT('',#8596);
#2573=VERTEX_POINT('',#8601);
#2574=VERTEX_POINT('',#8605);
#2575=VERTEX_POINT('',#8611);
#2576=VERTEX_POINT('',#8612);
#2577=VERTEX_POINT('',#8615);
#2578=VERTEX_POINT('',#8617);
#2579=VERTEX_POINT('',#8621);
#2580=VERTEX_POINT('',#8625);
#2581=VERTEX_POINT('',#8627);
#2582=VERTEX_POINT('',#8630);
#2583=VERTEX_POINT('',#8634);
#2584=VERTEX_POINT('',#8638);
#2585=VERTEX_POINT('',#8646);
#2586=VERTEX_POINT('',#8647);
#2587=VERTEX_POINT('',#8650);
#2588=VERTEX_POINT('',#8651);
#2589=VERTEX_POINT('',#8654);
#2590=VERTEX_POINT('',#8655);
#2591=VERTEX_POINT('',#8658);
#2592=VERTEX_POINT('',#8659);
#2593=VERTEX_POINT('',#8662);
#2594=VERTEX_POINT('',#8663);
#2595=VERTEX_POINT('',#8666);
#2596=VERTEX_POINT('',#8667);
#2597=VERTEX_POINT('',#8670);
#2598=VERTEX_POINT('',#8671);
#2599=VERTEX_POINT('',#8675);
#2600=VERTEX_POINT('',#8676);
#2601=VERTEX_POINT('',#8699);
#2602=VERTEX_POINT('',#8701);
#2603=VERTEX_POINT('',#8726);
#2604=VERTEX_POINT('',#8728);
#2605=VERTEX_POINT('',#8751);
#2606=VERTEX_POINT('',#8753);
#2607=VERTEX_POINT('',#8776);
#2608=VERTEX_POINT('',#8778);
#2609=VERTEX_POINT('',#8781);
#2610=VERTEX_POINT('',#8783);
#2611=VERTEX_POINT('',#8806);
#2612=VERTEX_POINT('',#8808);
#2613=VERTEX_POINT('',#8831);
#2614=VERTEX_POINT('',#8833);
#2615=VERTEX_POINT('',#8856);
#2616=VERTEX_POINT('',#8858);
#2617=VERTEX_POINT('',#8883);
#2618=VERTEX_POINT('',#8887);
#2619=VERTEX_POINT('',#8912);
#2620=VERTEX_POINT('',#8916);
#2621=VERTEX_POINT('',#8941);
#2622=VERTEX_POINT('',#8943);
#2623=VERTEX_POINT('',#8947);
#2624=VERTEX_POINT('',#8972);
#2625=VERTEX_POINT('',#8976);
#2626=VERTEX_POINT('',#9001);
#2627=VERTEX_POINT('',#9005);
#2628=VERTEX_POINT('',#9030);
#2629=VERTEX_POINT('',#9033);
#2630=VERTEX_POINT('',#9035);
#2631=VERTEX_POINT('',#9067);
#2632=VERTEX_POINT('',#9069);
#2633=VERTEX_POINT('',#9072);
#2634=VERTEX_POINT('',#9076);
#2635=VERTEX_POINT('',#9081);
#2636=VERTEX_POINT('',#9083);
#2637=VERTEX_POINT('',#9086);
#2638=VERTEX_POINT('',#9090);
#2639=VERTEX_POINT('',#9102);
#2640=VERTEX_POINT('',#9103);
#2641=VERTEX_POINT('',#9105);
#2642=VERTEX_POINT('',#9107);
#2643=VERTEX_POINT('',#9111);
#2644=VERTEX_POINT('',#9113);
#2645=VERTEX_POINT('',#9117);
#2646=VERTEX_POINT('',#9119);
#2647=VERTEX_POINT('',#9127);
#2648=VERTEX_POINT('',#9129);
#2649=VERTEX_POINT('',#9132);
#2650=VERTEX_POINT('',#9134);
#2651=VERTEX_POINT('',#9139);
#2652=VERTEX_POINT('',#9143);
#2653=VERTEX_POINT('',#9150);
#2654=VERTEX_POINT('',#9152);
#2655=VERTEX_POINT('',#9156);
#2656=VERTEX_POINT('',#9158);
#2657=VERTEX_POINT('',#9162);
#2658=VERTEX_POINT('',#9163);
#2659=VERTEX_POINT('',#9167);
#2660=VERTEX_POINT('',#9178);
#2661=VERTEX_POINT('',#9180);
#2662=VERTEX_POINT('',#9182);
#2663=VERTEX_POINT('',#9219);
#2664=VERTEX_POINT('',#9234);
#2665=VERTEX_POINT('',#9235);
#2666=VERTEX_POINT('',#9237);
#2667=VERTEX_POINT('',#9239);
#2668=VERTEX_POINT('',#9243);
#2669=VERTEX_POINT('',#9245);
#2670=VERTEX_POINT('',#9249);
#2671=VERTEX_POINT('',#9251);
#2672=VERTEX_POINT('',#9255);
#2673=VERTEX_POINT('',#9261);
#2674=VERTEX_POINT('',#9262);
#2675=VERTEX_POINT('',#9264);
#2676=VERTEX_POINT('',#9266);
#2677=VERTEX_POINT('',#9270);
#2678=VERTEX_POINT('',#9271);
#2679=VERTEX_POINT('',#9273);
#2680=VERTEX_POINT('',#9275);
#2681=VERTEX_POINT('',#9279);
#2682=VERTEX_POINT('',#9281);
#2683=VERTEX_POINT('',#9283);
#2684=VERTEX_POINT('',#9285);
#2685=VERTEX_POINT('',#9287);
#2686=VERTEX_POINT('',#9289);
#2687=VERTEX_POINT('',#9291);
#2688=VERTEX_POINT('',#9293);
#2689=VERTEX_POINT('',#9295);
#2690=VERTEX_POINT('',#9300);
#2691=VERTEX_POINT('',#9304);
#2692=VERTEX_POINT('',#9308);
#2693=VERTEX_POINT('',#9310);
#2694=VERTEX_POINT('',#9314);
#2695=VERTEX_POINT('',#9318);
#2696=VERTEX_POINT('',#9322);
#2697=VERTEX_POINT('',#9324);
#2698=VERTEX_POINT('',#9328);
#2699=VERTEX_POINT('',#9338);
#2700=VERTEX_POINT('',#9344);
#2701=VERTEX_POINT('',#9346);
#2702=VERTEX_POINT('',#9350);
#2703=VERTEX_POINT('',#9352);
#2704=VERTEX_POINT('',#9359);
#2705=VERTEX_POINT('',#9360);
#2706=VERTEX_POINT('',#9364);
#2707=VERTEX_POINT('',#9375);
#2708=VERTEX_POINT('',#9377);
#2709=VERTEX_POINT('',#9379);
#2710=VERTEX_POINT('',#9416);
#2711=VERTEX_POINT('',#9431);
#2712=VERTEX_POINT('',#9433);
#2713=VERTEX_POINT('',#9437);
#2714=VERTEX_POINT('',#9439);
#2715=VERTEX_POINT('',#9446);
#2716=VERTEX_POINT('',#9448);
#2717=VERTEX_POINT('',#9453);
#2718=VERTEX_POINT('',#9455);
#2719=VERTEX_POINT('',#9459);
#2720=VERTEX_POINT('',#9461);
#2721=VERTEX_POINT('',#9465);
#2722=VERTEX_POINT('',#9467);
#2723=VERTEX_POINT('',#9470);
#2724=VERTEX_POINT('',#9474);
#2725=VERTEX_POINT('',#9476);
#2726=VERTEX_POINT('',#9481);
#2727=VERTEX_POINT('',#9488);
#2728=VERTEX_POINT('',#9490);
#2729=VERTEX_POINT('',#9494);
#2730=VERTEX_POINT('',#9496);
#2731=VERTEX_POINT('',#9503);
#2732=VERTEX_POINT('',#9505);
#2733=VERTEX_POINT('',#9509);
#2734=VERTEX_POINT('',#9511);
#2735=VERTEX_POINT('',#9518);
#2736=VERTEX_POINT('',#9519);
#2737=VERTEX_POINT('',#9521);
#2738=VERTEX_POINT('',#9523);
#2739=VERTEX_POINT('',#9527);
#2740=VERTEX_POINT('',#9528);
#2741=VERTEX_POINT('',#9533);
#2742=VERTEX_POINT('',#9534);
#2743=VERTEX_POINT('',#9542);
#2744=VERTEX_POINT('',#9544);
#2745=VERTEX_POINT('',#9548);
#2746=VERTEX_POINT('',#9553);
#2747=VERTEX_POINT('',#9555);
#2748=VERTEX_POINT('',#9559);
#2749=VERTEX_POINT('',#9563);
#2750=VERTEX_POINT('',#9564);
#2751=VERTEX_POINT('',#9577);
#2752=VERTEX_POINT('',#9578);
#2753=VERTEX_POINT('',#9580);
#2754=VERTEX_POINT('',#9582);
#2755=VERTEX_POINT('',#9586);
#2756=VERTEX_POINT('',#9588);
#2757=VERTEX_POINT('',#9592);
#2758=VERTEX_POINT('',#9594);
#2759=VERTEX_POINT('',#9598);
#2760=VERTEX_POINT('',#9600);
#2761=VERTEX_POINT('',#9604);
#2762=VERTEX_POINT('',#9606);
#2763=VERTEX_POINT('',#9614);
#2764=VERTEX_POINT('',#9617);
#2765=VERTEX_POINT('',#9621);
#2766=VERTEX_POINT('',#9625);
#2767=VERTEX_POINT('',#9631);
#2768=VERTEX_POINT('',#9632);
#2769=VERTEX_POINT('',#9634);
#2770=VERTEX_POINT('',#9636);
#2771=VERTEX_POINT('',#9640);
#2772=VERTEX_POINT('',#9642);
#2773=VERTEX_POINT('',#9646);
#2774=VERTEX_POINT('',#9648);
#2775=VERTEX_POINT('',#9652);
#2776=VERTEX_POINT('',#9654);
#2777=VERTEX_POINT('',#9658);
#2778=VERTEX_POINT('',#9660);
#2779=VERTEX_POINT('',#9669);
#2780=VERTEX_POINT('',#9672);
#2781=VERTEX_POINT('',#9675);
#2782=VERTEX_POINT('',#9679);
#2783=VERTEX_POINT('',#9683);
#2784=VERTEX_POINT('',#9687);
#2785=VERTEX_POINT('',#9690);
#2786=VERTEX_POINT('',#9698);
#2787=VERTEX_POINT('',#9699);
#2788=VERTEX_POINT('',#9702);
#2789=VERTEX_POINT('',#9704);
#2790=VERTEX_POINT('',#9708);
#2791=VERTEX_POINT('',#9712);
#2792=VERTEX_POINT('',#9714);
#2793=VERTEX_POINT('',#9718);
#2794=VERTEX_POINT('',#9723);
#2795=VERTEX_POINT('',#9727);
#2796=VERTEX_POINT('',#9733);
#2797=VERTEX_POINT('',#9734);
#2798=VERTEX_POINT('',#9737);
#2799=VERTEX_POINT('',#9739);
#2800=VERTEX_POINT('',#9743);
#2801=VERTEX_POINT('',#9747);
#2802=VERTEX_POINT('',#9749);
#2803=VERTEX_POINT('',#9752);
#2804=VERTEX_POINT('',#9756);
#2805=VERTEX_POINT('',#9760);
#2806=VERTEX_POINT('',#9768);
#2807=VERTEX_POINT('',#9769);
#2808=VERTEX_POINT('',#9772);
#2809=VERTEX_POINT('',#9773);
#2810=VERTEX_POINT('',#9776);
#2811=VERTEX_POINT('',#9777);
#2812=VERTEX_POINT('',#9780);
#2813=VERTEX_POINT('',#9781);
#2814=VERTEX_POINT('',#9784);
#2815=VERTEX_POINT('',#9785);
#2816=VERTEX_POINT('',#9788);
#2817=VERTEX_POINT('',#9789);
#2818=VERTEX_POINT('',#9792);
#2819=VERTEX_POINT('',#9793);
#2820=VERTEX_POINT('',#9796);
#2821=VERTEX_POINT('',#9797);
#2822=VERTEX_POINT('',#9801);
#2823=VERTEX_POINT('',#9802);
#2824=VERTEX_POINT('',#9825);
#2825=VERTEX_POINT('',#9827);
#2826=VERTEX_POINT('',#9852);
#2827=VERTEX_POINT('',#9854);
#2828=VERTEX_POINT('',#9877);
#2829=VERTEX_POINT('',#9879);
#2830=VERTEX_POINT('',#9902);
#2831=VERTEX_POINT('',#9904);
#2832=VERTEX_POINT('',#9917);
#2833=VERTEX_POINT('',#9920);
#2834=VERTEX_POINT('',#9933);
#2835=VERTEX_POINT('',#9935);
#2836=VERTEX_POINT('',#9958);
#2837=VERTEX_POINT('',#9960);
#2838=VERTEX_POINT('',#9983);
#2839=VERTEX_POINT('',#9985);
#2840=VERTEX_POINT('',#10008);
#2841=VERTEX_POINT('',#10010);
#2842=VERTEX_POINT('',#10035);
#2843=VERTEX_POINT('',#10039);
#2844=VERTEX_POINT('',#10064);
#2845=VERTEX_POINT('',#10068);
#2846=VERTEX_POINT('',#10093);
#2847=VERTEX_POINT('',#10097);
#2848=VERTEX_POINT('',#10098);
#2849=VERTEX_POINT('',#10125);
#2850=VERTEX_POINT('',#10129);
#2851=VERTEX_POINT('',#10154);
#2852=VERTEX_POINT('',#10158);
#2853=VERTEX_POINT('',#10183);
#2854=VERTEX_POINT('',#10187);
#2855=VERTEX_POINT('',#10212);
#2856=VERTEX_POINT('',#10215);
#2857=VERTEX_POINT('',#10217);
#2858=VERTEX_POINT('',#10249);
#2859=VERTEX_POINT('',#10251);
#2860=VERTEX_POINT('',#10254);
#2861=VERTEX_POINT('',#10258);
#2862=VERTEX_POINT('',#10263);
#2863=VERTEX_POINT('',#10265);
#2864=VERTEX_POINT('',#10268);
#2865=VERTEX_POINT('',#10272);
#2866=VERTEX_POINT('',#10283);
#2867=VERTEX_POINT('',#10286);
#2868=VERTEX_POINT('',#10290);
#2869=VERTEX_POINT('',#10294);
#2870=VERTEX_POINT('',#10298);
#2871=VERTEX_POINT('',#10301);
#2872=VERTEX_POINT('',#10305);
#2873=VERTEX_POINT('',#10309);
#2874=VERTEX_POINT('',#10314);
#2875=VERTEX_POINT('',#10315);
#2876=VERTEX_POINT('',#10317);
#2877=VERTEX_POINT('',#10319);
#2878=VERTEX_POINT('',#10323);
#2879=VERTEX_POINT('',#10325);
#2880=VERTEX_POINT('',#10329);
#2881=VERTEX_POINT('',#10331);
#2882=VERTEX_POINT('',#10335);
#2883=VERTEX_POINT('',#10337);
#2884=VERTEX_POINT('',#10341);
#2885=VERTEX_POINT('',#10343);
#2886=VERTEX_POINT('',#10393);
#2887=VERTEX_POINT('',#10395);
#2888=VERTEX_POINT('',#10399);
#2889=VERTEX_POINT('',#10402);
#2890=VERTEX_POINT('',#10406);
#2891=VERTEX_POINT('',#10408);
#2892=VERTEX_POINT('',#10415);
#2893=VERTEX_POINT('',#10417);
#2894=VERTEX_POINT('',#10421);
#2895=VERTEX_POINT('',#10423);
#2896=EDGE_CURVE('',#2444,#2444,#2133,.T.);
#2897=EDGE_CURVE('',#2444,#2445,#1513,.T.);
#2898=EDGE_CURVE('',#2445,#2445,#2134,.T.);
#2899=EDGE_CURVE('',#2446,#2446,#2135,.T.);
#2900=EDGE_CURVE('',#2446,#2447,#1514,.T.);
#2901=EDGE_CURVE('',#2447,#2447,#2136,.T.);
#2902=EDGE_CURVE('',#2448,#2448,#2137,.T.);
#2903=EDGE_CURVE('',#2448,#2449,#1515,.T.);
#2904=EDGE_CURVE('',#2449,#2449,#2138,.T.);
#2905=EDGE_CURVE('',#2450,#2450,#2139,.T.);
#2906=EDGE_CURVE('',#2450,#2451,#1516,.T.);
#2907=EDGE_CURVE('',#2451,#2451,#2140,.T.);
#2908=EDGE_CURVE('',#2452,#2453,#1517,.T.);
#2909=EDGE_CURVE('',#2453,#2454,#1518,.T.);
#2910=EDGE_CURVE('',#2455,#2454,#1519,.T.);
#2911=EDGE_CURVE('',#2452,#2455,#1520,.T.);
#2912=EDGE_CURVE('',#2456,#2452,#1521,.T.);
#2913=EDGE_CURVE('',#2457,#2455,#1522,.T.);
#2914=EDGE_CURVE('',#2456,#2457,#1523,.T.);
#2915=EDGE_CURVE('',#2458,#2456,#1524,.T.);
#2916=EDGE_CURVE('',#2459,#2457,#1525,.T.);
#2917=EDGE_CURVE('',#2458,#2459,#1526,.T.);
#2918=EDGE_CURVE('',#2453,#2458,#1527,.T.);
#2919=EDGE_CURVE('',#2454,#2459,#1528,.T.);
#2920=EDGE_CURVE('',#2460,#2461,#1529,.T.);
#2921=EDGE_CURVE('',#2461,#2462,#1530,.T.);
#2922=EDGE_CURVE('',#2463,#2462,#1531,.T.);
#2923=EDGE_CURVE('',#2460,#2463,#1532,.T.);
#2924=EDGE_CURVE('',#2464,#2460,#1533,.T.);
#2925=EDGE_CURVE('',#2465,#2463,#1534,.T.);
#2926=EDGE_CURVE('',#2464,#2465,#1535,.T.);
#2927=EDGE_CURVE('',#2466,#2464,#1536,.T.);
#2928=EDGE_CURVE('',#2467,#2465,#1537,.T.);
#2929=EDGE_CURVE('',#2466,#2467,#1538,.T.);
#2930=EDGE_CURVE('',#2461,#2466,#1539,.T.);
#2931=EDGE_CURVE('',#2462,#2467,#1540,.T.);
#2932=EDGE_CURVE('',#2468,#2469,#1541,.T.);
#2933=EDGE_CURVE('',#2469,#2470,#1542,.T.);
#2934=EDGE_CURVE('',#2471,#2470,#1543,.T.);
#2935=EDGE_CURVE('',#2468,#2471,#1544,.T.);
#2936=EDGE_CURVE('',#2472,#2468,#1545,.T.);
#2937=EDGE_CURVE('',#2473,#2471,#1546,.T.);
#2938=EDGE_CURVE('',#2472,#2473,#1547,.T.);
#2939=EDGE_CURVE('',#2474,#2472,#1548,.T.);
#2940=EDGE_CURVE('',#2475,#2473,#1549,.T.);
#2941=EDGE_CURVE('',#2474,#2475,#1550,.T.);
#2942=EDGE_CURVE('',#2469,#2474,#1551,.T.);
#2943=EDGE_CURVE('',#2470,#2475,#1552,.T.);
#2944=EDGE_CURVE('',#2476,#2476,#2141,.T.);
#2945=EDGE_CURVE('',#2476,#2477,#1553,.T.);
#2946=EDGE_CURVE('',#2477,#2477,#2142,.T.);
#2947=EDGE_CURVE('',#2478,#2478,#2143,.T.);
#2948=EDGE_CURVE('',#2478,#2479,#1554,.T.);
#2949=EDGE_CURVE('',#2479,#2479,#2144,.T.);
#2950=EDGE_CURVE('',#2480,#2480,#2145,.T.);
#2951=EDGE_CURVE('',#2480,#2481,#1555,.T.);
#2952=EDGE_CURVE('',#2481,#2481,#2146,.T.);
#2953=EDGE_CURVE('',#2482,#2482,#2147,.T.);
#2954=EDGE_CURVE('',#2482,#2483,#1556,.T.);
#2955=EDGE_CURVE('',#2483,#2483,#2148,.T.);
#2956=EDGE_CURVE('',#2484,#2484,#2149,.T.);
#2957=EDGE_CURVE('',#2484,#2485,#1557,.T.);
#2958=EDGE_CURVE('',#2485,#2485,#2150,.T.);
#2959=EDGE_CURVE('',#2486,#2486,#2151,.T.);
#2960=EDGE_CURVE('',#2486,#2487,#1558,.T.);
#2961=EDGE_CURVE('',#2487,#2487,#2152,.T.);
#2962=EDGE_CURVE('',#2488,#2488,#2153,.T.);
#2963=EDGE_CURVE('',#2488,#2489,#1559,.T.);
#2964=EDGE_CURVE('',#2489,#2489,#2154,.T.);
#2965=EDGE_CURVE('',#2490,#2490,#2155,.T.);
#2966=EDGE_CURVE('',#2490,#2491,#1560,.T.);
#2967=EDGE_CURVE('',#2491,#2491,#2156,.T.);
#2968=EDGE_CURVE('',#2492,#2492,#2157,.T.);
#2969=EDGE_CURVE('',#2492,#2493,#1561,.T.);
#2970=EDGE_CURVE('',#2493,#2493,#2158,.T.);
#2971=EDGE_CURVE('',#2494,#2495,#1562,.T.);
#2972=EDGE_CURVE('',#2496,#2494,#1563,.T.);
#2973=EDGE_CURVE('',#2496,#2497,#1564,.T.);
#2974=EDGE_CURVE('',#2495,#2497,#1565,.T.);
#2975=EDGE_CURVE('',#2498,#2499,#1566,.T.);
#2976=EDGE_CURVE('',#2500,#2498,#1567,.T.);
#2977=EDGE_CURVE('',#2501,#2500,#1568,.T.);
#2978=EDGE_CURVE('',#2499,#2501,#1569,.T.);
#2979=EDGE_CURVE('',#2501,#2502,#1570,.T.);
#2980=EDGE_CURVE('',#2503,#2500,#1571,.T.);
#2981=EDGE_CURVE('',#2502,#2503,#1572,.T.);
#2982=EDGE_CURVE('',#2504,#2496,#1573,.T.);
#2983=EDGE_CURVE('',#2504,#2505,#1574,.T.);
#2984=EDGE_CURVE('',#2497,#2505,#1575,.T.);
#2985=EDGE_CURVE('',#2494,#2506,#1576,.T.);
#2986=EDGE_CURVE('',#2507,#2506,#1577,.T.);
#2987=EDGE_CURVE('',#2499,#2507,#1578,.T.);
#2988=EDGE_CURVE('',#2502,#2504,#1579,.T.);
#2989=EDGE_CURVE('',#2495,#2508,#1580,.T.);
#2990=EDGE_CURVE('',#2506,#2508,#1581,.T.);
#2991=EDGE_CURVE('',#2498,#2509,#1582,.T.);
#2992=EDGE_CURVE('',#2508,#2509,#1583,.T.);
#2993=EDGE_CURVE('',#2505,#2503,#1584,.T.);
#2994=EDGE_CURVE('',#2509,#2507,#1585,.T.);
#2995=EDGE_CURVE('',#2510,#2510,#2159,.T.);
#2996=EDGE_CURVE('',#2510,#2511,#1586,.T.);
#2997=EDGE_CURVE('',#2511,#2511,#2160,.T.);
#2998=EDGE_CURVE('',#2512,#2512,#2161,.T.);
#2999=EDGE_CURVE('',#2512,#2513,#1587,.T.);
#3000=EDGE_CURVE('',#2513,#2513,#2162,.T.);
#3001=EDGE_CURVE('',#2514,#2514,#2163,.T.);
#3002=EDGE_CURVE('',#2514,#2515,#1588,.T.);
#3003=EDGE_CURVE('',#2515,#2515,#2164,.T.);
#3004=EDGE_CURVE('',#2516,#2516,#2165,.T.);
#3005=EDGE_CURVE('',#2516,#2517,#1589,.T.);
#3006=EDGE_CURVE('',#2517,#2517,#2166,.T.);
#3007=EDGE_CURVE('',#2518,#2518,#2167,.T.);
#3008=EDGE_CURVE('',#2518,#2519,#1590,.T.);
#3009=EDGE_CURVE('',#2519,#2519,#2168,.T.);
#3010=EDGE_CURVE('',#2520,#2520,#2169,.T.);
#3011=EDGE_CURVE('',#2520,#2521,#1591,.T.);
#3012=EDGE_CURVE('',#2521,#2521,#2170,.T.);
#3013=EDGE_CURVE('',#2522,#2522,#2171,.T.);
#3014=EDGE_CURVE('',#2522,#2523,#1592,.T.);
#3015=EDGE_CURVE('',#2523,#2523,#2172,.T.);
#3016=EDGE_CURVE('',#2524,#2524,#2173,.T.);
#3017=EDGE_CURVE('',#2524,#2525,#1593,.T.);
#3018=EDGE_CURVE('',#2525,#2525,#2174,.T.);
#3019=EDGE_CURVE('',#2526,#2526,#2175,.T.);
#3020=EDGE_CURVE('',#2526,#2527,#1594,.T.);
#3021=EDGE_CURVE('',#2527,#2527,#2176,.T.);
#3022=EDGE_CURVE('',#2528,#2528,#2177,.T.);
#3023=EDGE_CURVE('',#2528,#2529,#1595,.T.);
#3024=EDGE_CURVE('',#2529,#2529,#2178,.T.);
#3025=EDGE_CURVE('',#2530,#2530,#2179,.T.);
#3026=EDGE_CURVE('',#2530,#2531,#1596,.T.);
#3027=EDGE_CURVE('',#2531,#2531,#2180,.T.);
#3028=EDGE_CURVE('',#2532,#2532,#2181,.T.);
#3029=EDGE_CURVE('',#2532,#2533,#1597,.T.);
#3030=EDGE_CURVE('',#2533,#2533,#2182,.T.);
#3031=EDGE_CURVE('',#2534,#2534,#2183,.T.);
#3032=EDGE_CURVE('',#2534,#2535,#1598,.T.);
#3033=EDGE_CURVE('',#2535,#2535,#2184,.T.);
#3034=EDGE_CURVE('',#2536,#2536,#2185,.T.);
#3035=EDGE_CURVE('',#2536,#2537,#1599,.T.);
#3036=EDGE_CURVE('',#2537,#2537,#2186,.T.);
#3037=EDGE_CURVE('',#2538,#2538,#2187,.T.);
#3038=EDGE_CURVE('',#2539,#2539,#2188,.T.);
#3039=EDGE_CURVE('',#2539,#2538,#1600,.T.);
#3040=EDGE_CURVE('',#2540,#2540,#2189,.T.);
#3041=EDGE_CURVE('',#2540,#2541,#1601,.T.);
#3042=EDGE_CURVE('',#2541,#2541,#2190,.T.);
#3043=EDGE_CURVE('',#2542,#2542,#2191,.T.);
#3044=EDGE_CURVE('',#2542,#2543,#1602,.T.);
#3045=EDGE_CURVE('',#2543,#2543,#2192,.T.);
#3046=EDGE_CURVE('',#2544,#2544,#2193,.T.);
#3047=EDGE_CURVE('',#2544,#2545,#1603,.T.);
#3048=EDGE_CURVE('',#2545,#2545,#2194,.T.);
#3049=EDGE_CURVE('',#2546,#2547,#1604,.T.);
#3050=EDGE_CURVE('',#2547,#2548,#1605,.T.);
#3051=EDGE_CURVE('',#2548,#2549,#1606,.T.);
#3052=EDGE_CURVE('',#2546,#2549,#1607,.T.);
#3053=EDGE_CURVE('',#2547,#2550,#1608,.T.);
#3054=EDGE_CURVE('',#2550,#2551,#1609,.T.);
#3055=EDGE_CURVE('',#2551,#2548,#1610,.T.);
#3056=EDGE_CURVE('',#2550,#2552,#1611,.T.);
#3057=EDGE_CURVE('',#2552,#2553,#1612,.T.);
#3058=EDGE_CURVE('',#2553,#2551,#1613,.T.);
#3059=EDGE_CURVE('',#2552,#2554,#1614,.T.);
#3060=EDGE_CURVE('',#2554,#2555,#1615,.T.);
#3061=EDGE_CURVE('',#2555,#2553,#1616,.T.);
#3062=EDGE_CURVE('',#2554,#2556,#1617,.T.);
#3063=EDGE_CURVE('',#2556,#2557,#1618,.T.);
#3064=EDGE_CURVE('',#2557,#2555,#1619,.T.);
#3065=EDGE_CURVE('',#2556,#2546,#1620,.T.);
#3066=EDGE_CURVE('',#2549,#2557,#1621,.T.);
#3067=EDGE_CURVE('',#2558,#2558,#2195,.T.);
#3068=EDGE_CURVE('',#2559,#2559,#2196,.T.);
#3069=EDGE_CURVE('',#2560,#2560,#2197,.T.);
#3070=EDGE_CURVE('',#2560,#2559,#1622,.T.);
#3071=EDGE_CURVE('',#2561,#2561,#2198,.T.);
#3072=EDGE_CURVE('',#2561,#2560,#1623,.T.);
#3073=EDGE_CURVE('',#2562,#2562,#2199,.T.);
#3074=EDGE_CURVE('',#2562,#2561,#1624,.T.);
#3075=EDGE_CURVE('',#2563,#2563,#2200,.T.);
#3076=EDGE_CURVE('',#2564,#2564,#2201,.F.);
#3077=EDGE_CURVE('',#2564,#2563,#1625,.T.);
#3078=EDGE_CURVE('',#2558,#2564,#1626,.T.);
#3079=EDGE_CURVE('',#2565,#2566,#2202,.T.);
#3080=EDGE_CURVE('',#2566,#2565,#2203,.T.);
#3081=EDGE_CURVE('',#2566,#2567,#2204,.T.);
#3082=EDGE_CURVE('',#2568,#2567,#2205,.T.);
#3083=EDGE_CURVE('',#2567,#2568,#2206,.T.);
#3084=EDGE_CURVE('',#2568,#2569,#1627,.T.);
#3085=EDGE_CURVE('',#2569,#2569,#2207,.T.);
#3086=EDGE_CURVE('',#2570,#2570,#2208,.T.);
#3087=EDGE_CURVE('',#2570,#2571,#1628,.T.);
#3088=EDGE_CURVE('',#2571,#2571,#2209,.T.);
#3089=EDGE_CURVE('',#2571,#2572,#1629,.T.);
#3090=EDGE_CURVE('',#2572,#2572,#2210,.T.);
#3091=EDGE_CURVE('',#2573,#2573,#2211,.T.);
#3092=EDGE_CURVE('',#2573,#2565,#1630,.T.);
#3093=EDGE_CURVE('',#2574,#2574,#2212,.T.);
#3094=EDGE_CURVE('',#2574,#2570,#1631,.T.);
#3095=EDGE_CURVE('',#2575,#2576,#2213,.T.);
#3096=EDGE_CURVE('',#2576,#2575,#2214,.T.);
#3097=EDGE_CURVE('',#2576,#2577,#2215,.T.);
#3098=EDGE_CURVE('',#2578,#2577,#2216,.T.);
#3099=EDGE_CURVE('',#2577,#2578,#2217,.T.);
#3100=EDGE_CURVE('',#2579,#2579,#2218,.T.);
#3101=EDGE_CURVE('',#2579,#2578,#1632,.T.);
#3102=EDGE_CURVE('',#2580,#2580,#2219,.T.);
#3103=EDGE_CURVE('',#2581,#2581,#2220,.T.);
#3104=EDGE_CURVE('',#2582,#2582,#2221,.T.);
#3105=EDGE_CURVE('',#2582,#2580,#1633,.T.);
#3106=EDGE_CURVE('',#2583,#2583,#2222,.T.);
#3107=EDGE_CURVE('',#2583,#2582,#1634,.T.);
#3108=EDGE_CURVE('',#2584,#2584,#2223,.T.);
#3109=EDGE_CURVE('',#2584,#2583,#1635,.T.);
#3110=EDGE_CURVE('',#2575,#2581,#1636,.T.);
#3111=EDGE_CURVE('',#2585,#2586,#2224,.T.);
#3112=EDGE_CURVE('',#2587,#2588,#2225,.T.);
#3113=EDGE_CURVE('',#2589,#2590,#2226,.T.);
#3114=EDGE_CURVE('',#2591,#2592,#2227,.T.);
#3115=EDGE_CURVE('',#2593,#2594,#2228,.T.);
#3116=EDGE_CURVE('',#2595,#2596,#2229,.T.);
#3117=EDGE_CURVE('',#2597,#2598,#2230,.T.);
#3118=EDGE_CURVE('',#2599,#2600,#227,.T.);
#3119=EDGE_CURVE('',#2601,#2599,#2231,.T.);
#3120=EDGE_CURVE('',#2602,#2601,#228,.T.);
#3121=EDGE_CURVE('',#2600,#2602,#2232,.T.);
#3122=EDGE_CURVE('',#2603,#2601,#2233,.T.);
#3123=EDGE_CURVE('',#2603,#2604,#229,.T.);
#3124=EDGE_CURVE('',#2605,#2604,#2234,.T.);
#3125=EDGE_CURVE('',#2605,#2606,#230,.T.);
#3126=EDGE_CURVE('',#2607,#2606,#2235,.T.);
#3127=EDGE_CURVE('',#2607,#2608,#1637,.T.);
#3128=EDGE_CURVE('',#2608,#2608,#2236,.T.);
#3129=EDGE_CURVE('',#2609,#2607,#2237,.T.);
#3130=EDGE_CURVE('',#2609,#2610,#231,.T.);
#3131=EDGE_CURVE('',#2611,#2610,#2238,.T.);
#3132=EDGE_CURVE('',#2611,#2612,#232,.T.);
#3133=EDGE_CURVE('',#2613,#2612,#2239,.T.);
#3134=EDGE_CURVE('',#2613,#2614,#233,.T.);
#3135=EDGE_CURVE('',#2615,#2614,#2240,.T.);
#3136=EDGE_CURVE('',#2615,#2616,#234,.T.);
#3137=EDGE_CURVE('',#2602,#2616,#2241,.T.);
#3138=EDGE_CURVE('',#2599,#2617,#2242,.T.);
#3139=EDGE_CURVE('',#2617,#2603,#2243,.T.);
#3140=EDGE_CURVE('',#2618,#2617,#235,.T.);
#3141=EDGE_CURVE('',#2604,#2618,#2244,.T.);
#3142=EDGE_CURVE('',#2618,#2619,#2245,.T.);
#3143=EDGE_CURVE('',#2619,#2605,#2246,.T.);
#3144=EDGE_CURVE('',#2620,#2619,#236,.T.);
#3145=EDGE_CURVE('',#2606,#2620,#2247,.T.);
#3146=EDGE_CURVE('',#2620,#2621,#2248,.T.);
#3147=EDGE_CURVE('',#2621,#2622,#2249,.T.);
#3148=EDGE_CURVE('',#2622,#2609,#2250,.T.);
#3149=EDGE_CURVE('',#2623,#2622,#237,.T.);
#3150=EDGE_CURVE('',#2610,#2623,#2251,.T.);
#3151=EDGE_CURVE('',#2623,#2624,#2252,.T.);
#3152=EDGE_CURVE('',#2624,#2611,#2253,.T.);
#3153=EDGE_CURVE('',#2625,#2624,#238,.T.);
#3154=EDGE_CURVE('',#2612,#2625,#2254,.T.);
#3155=EDGE_CURVE('',#2625,#2626,#2255,.T.);
#3156=EDGE_CURVE('',#2626,#2613,#2256,.T.);
#3157=EDGE_CURVE('',#2627,#2626,#239,.T.);
#3158=EDGE_CURVE('',#2614,#2627,#2257,.T.);
#3159=EDGE_CURVE('',#2628,#2628,#2258,.T.);
#3160=EDGE_CURVE('',#2628,#2621,#1638,.T.);
#3161=EDGE_CURVE('',#2629,#2600,#2259,.T.);
#3162=EDGE_CURVE('',#2629,#2630,#240,.T.);
#3163=EDGE_CURVE('',#2627,#2630,#2260,.T.);
#3164=EDGE_CURVE('',#2616,#2629,#2261,.T.);
#3165=EDGE_CURVE('',#2630,#2615,#2262,.T.);
#3166=EDGE_CURVE('',#2631,#2631,#2263,.T.);
#3167=EDGE_CURVE('',#2632,#2632,#2264,.T.);
#3168=EDGE_CURVE('',#2633,#2633,#2265,.T.);
#3169=EDGE_CURVE('',#2633,#2631,#1639,.T.);
#3170=EDGE_CURVE('',#2634,#2634,#2266,.T.);
#3171=EDGE_CURVE('',#2634,#2632,#1640,.T.);
#3172=EDGE_CURVE('',#2635,#2635,#2267,.T.);
#3173=EDGE_CURVE('',#2636,#2636,#2268,.T.);
#3174=EDGE_CURVE('',#2637,#2637,#2269,.T.);
#3175=EDGE_CURVE('',#2637,#2635,#1641,.T.);
#3176=EDGE_CURVE('',#2638,#2638,#2270,.T.);
#3177=EDGE_CURVE('',#2638,#2636,#1642,.T.);
#3178=EDGE_CURVE('',#2639,#2640,#1643,.T.);
#3179=EDGE_CURVE('',#2639,#2641,#1644,.T.);
#3180=EDGE_CURVE('',#2642,#2641,#1645,.T.);
#3181=EDGE_CURVE('',#2642,#2640,#1646,.T.);
#3182=EDGE_CURVE('',#2640,#2643,#2271,.T.);
#3183=EDGE_CURVE('',#2644,#2642,#1647,.T.);
#3184=EDGE_CURVE('',#2643,#2644,#1648,.T.);
#3185=EDGE_CURVE('',#2643,#2645,#1649,.T.);
#3186=EDGE_CURVE('',#2644,#2646,#1650,.T.);
#3187=EDGE_CURVE('',#2646,#2645,#1651,.T.);
#3188=EDGE_CURVE('',#2641,#2646,#1652,.T.);
#3189=EDGE_CURVE('',#2645,#2639,#2272,.T.);
#3190=EDGE_CURVE('',#2647,#2647,#2273,.T.);
#3191=EDGE_CURVE('',#2648,#2648,#2274,.T.);
#3192=EDGE_CURVE('',#2649,#2649,#2275,.T.);
#3193=EDGE_CURVE('',#2650,#2650,#2276,.T.);
#3194=EDGE_CURVE('',#2647,#2649,#1653,.T.);
#3195=EDGE_CURVE('',#2650,#2651,#1654,.T.);
#3196=EDGE_CURVE('',#2651,#2651,#2277,.T.);
#3197=EDGE_CURVE('',#2652,#2652,#2278,.T.);
#3198=EDGE_CURVE('',#2652,#2648,#1655,.T.);
#3199=EDGE_CURVE('',#2653,#2653,#2279,.T.);
#3200=EDGE_CURVE('',#2653,#2654,#1656,.T.);
#3201=EDGE_CURVE('',#2654,#2654,#2280,.T.);
#3202=EDGE_CURVE('',#2655,#2655,#2281,.T.);
#3203=EDGE_CURVE('',#2655,#2656,#1657,.T.);
#3204=EDGE_CURVE('',#2656,#2656,#2282,.T.);
#3205=EDGE_CURVE('',#2657,#2658,#1658,.T.);
#3206=EDGE_CURVE('',#2657,#2658,#2283,.T.);
#3207=EDGE_CURVE('',#2659,#2657,#241,.T.);
#3208=EDGE_CURVE('',#2660,#2659,#2284,.T.);
#3209=EDGE_CURVE('',#2660,#2661,#1659,.T.);
#3210=EDGE_CURVE('',#2662,#2661,#242,.T.);
#3211=EDGE_CURVE('',#2661,#2662,#243,.T.);
#3212=EDGE_CURVE('',#2663,#2660,#2285,.T.);
#3213=EDGE_CURVE('',#2658,#2663,#244,.T.);
#3214=EDGE_CURVE('',#2663,#2659,#1660,.T.);
#3215=EDGE_CURVE('',#2664,#2665,#1661,.T.);
#3216=EDGE_CURVE('',#2664,#2666,#1662,.T.);
#3217=EDGE_CURVE('',#2667,#2666,#1663,.T.);
#3218=EDGE_CURVE('',#2665,#2667,#1664,.T.);
#3219=EDGE_CURVE('',#2668,#2664,#1665,.T.);
#3220=EDGE_CURVE('',#2668,#2669,#1666,.T.);
#3221=EDGE_CURVE('',#2666,#2669,#1667,.T.);
#3222=EDGE_CURVE('',#2670,#2668,#1668,.T.);
#3223=EDGE_CURVE('',#2671,#2670,#1669,.T.);
#3224=EDGE_CURVE('',#2669,#2671,#1670,.T.);
#3225=EDGE_CURVE('',#2672,#2672,#2286,.T.);
#3226=EDGE_CURVE('',#2671,#2667,#2287,.T.);
#3227=EDGE_CURVE('',#2670,#2665,#2288,.T.);
#3228=EDGE_CURVE('',#2673,#2674,#1671,.T.);
#3229=EDGE_CURVE('',#2675,#2673,#1672,.T.);
#3230=EDGE_CURVE('',#2676,#2675,#1673,.T.);
#3231=EDGE_CURVE('',#2674,#2676,#1674,.T.);
#3232=EDGE_CURVE('',#2677,#2678,#1675,.T.);
#3233=EDGE_CURVE('',#2679,#2677,#1676,.T.);
#3234=EDGE_CURVE('',#2680,#2679,#1677,.T.);
#3235=EDGE_CURVE('',#2678,#2680,#1678,.T.);
#3236=EDGE_CURVE('',#2681,#2681,#2289,.T.);
#3237=EDGE_CURVE('',#2682,#2677,#2290,.T.);
#3238=EDGE_CURVE('',#2682,#2683,#1679,.T.);
#3239=EDGE_CURVE('',#2684,#2683,#2291,.T.);
#3240=EDGE_CURVE('',#2684,#2685,#1680,.T.);
#3241=EDGE_CURVE('',#2686,#2685,#2292,.T.);
#3242=EDGE_CURVE('',#2686,#2687,#1681,.T.);
#3243=EDGE_CURVE('',#2688,#2687,#2293,.T.);
#3244=EDGE_CURVE('',#2688,#2689,#1682,.T.);
#3245=EDGE_CURVE('',#2674,#2689,#2294,.T.);
#3246=EDGE_CURVE('',#2679,#2676,#2295,.T.);
#3247=EDGE_CURVE('',#2690,#2678,#2296,.T.);
#3248=EDGE_CURVE('',#2690,#2682,#1683,.T.);
#3249=EDGE_CURVE('',#2691,#2690,#1684,.T.);
#3250=EDGE_CURVE('',#2683,#2691,#1685,.T.);
#3251=EDGE_CURVE('',#2685,#2692,#1686,.T.);
#3252=EDGE_CURVE('',#2693,#2684,#1687,.T.);
#3253=EDGE_CURVE('',#2692,#2693,#1688,.T.);
#3254=EDGE_CURVE('',#2694,#2692,#2297,.T.);
#3255=EDGE_CURVE('',#2694,#2686,#1689,.T.);
#3256=EDGE_CURVE('',#2687,#2695,#1690,.T.);
#3257=EDGE_CURVE('',#2695,#2694,#1691,.T.);
#3258=EDGE_CURVE('',#2696,#2688,#1692,.T.);
#3259=EDGE_CURVE('',#2697,#2696,#1693,.T.);
#3260=EDGE_CURVE('',#2689,#2697,#1694,.T.);
#3261=EDGE_CURVE('',#2698,#2698,#2298,.T.);
#3262=EDGE_CURVE('',#2673,#2697,#2299,.T.);
#3263=EDGE_CURVE('',#2695,#2696,#2300,.T.);
#3264=EDGE_CURVE('',#2691,#2693,#2301,.T.);
#3265=EDGE_CURVE('',#2675,#2680,#2302,.T.);
#3266=EDGE_CURVE('',#2698,#2681,#1695,.T.);
#3267=EDGE_CURVE('',#2672,#2699,#1696,.T.);
#3268=EDGE_CURVE('',#2699,#2699,#2303,.T.);
#3269=EDGE_CURVE('',#2700,#2700,#2304,.T.);
#3270=EDGE_CURVE('',#2700,#2701,#1697,.T.);
#3271=EDGE_CURVE('',#2701,#2701,#2305,.T.);
#3272=EDGE_CURVE('',#2702,#2702,#2306,.T.);
#3273=EDGE_CURVE('',#2702,#2703,#1698,.T.);
#3274=EDGE_CURVE('',#2703,#2703,#2307,.T.);
#3275=EDGE_CURVE('',#2704,#2705,#1699,.T.);
#3276=EDGE_CURVE('',#2704,#2705,#2308,.T.);
#3277=EDGE_CURVE('',#2706,#2704,#245,.T.);
#3278=EDGE_CURVE('',#2707,#2706,#2309,.T.);
#3279=EDGE_CURVE('',#2707,#2708,#1700,.T.);
#3280=EDGE_CURVE('',#2709,#2708,#246,.T.);
#3281=EDGE_CURVE('',#2708,#2709,#247,.T.);
#3282=EDGE_CURVE('',#2710,#2707,#2310,.T.);
#3283=EDGE_CURVE('',#2705,#2710,#248,.T.);
#3284=EDGE_CURVE('',#2710,#2706,#1701,.T.);
#3285=EDGE_CURVE('',#2711,#2711,#2311,.T.);
#3286=EDGE_CURVE('',#2711,#2712,#1702,.T.);
#3287=EDGE_CURVE('',#2712,#2712,#2312,.T.);
#3288=EDGE_CURVE('',#2713,#2713,#2313,.T.);
#3289=EDGE_CURVE('',#2713,#2714,#1703,.T.);
#3290=EDGE_CURVE('',#2714,#2714,#2314,.T.);
#3291=EDGE_CURVE('',#2715,#2715,#2315,.T.);
#3292=EDGE_CURVE('',#2715,#2716,#1704,.T.);
#3293=EDGE_CURVE('',#2716,#2716,#2316,.T.);
#3294=EDGE_CURVE('',#2717,#2717,#2317,.T.);
#3295=EDGE_CURVE('',#2717,#2718,#1705,.T.);
#3296=EDGE_CURVE('',#2718,#2718,#2318,.T.);
#3297=EDGE_CURVE('',#2719,#2719,#2319,.T.);
#3298=EDGE_CURVE('',#2719,#2720,#1706,.T.);
#3299=EDGE_CURVE('',#2720,#2720,#2320,.T.);
#3300=EDGE_CURVE('',#2721,#2721,#2321,.T.);
#3301=EDGE_CURVE('',#2722,#2722,#2322,.T.);
#3302=EDGE_CURVE('',#2723,#2723,#2323,.T.);
#3303=EDGE_CURVE('',#2723,#2721,#1707,.T.);
#3304=EDGE_CURVE('',#2724,#2724,#2324,.T.);
#3305=EDGE_CURVE('',#2725,#2725,#2325,.T.);
#3306=EDGE_CURVE('',#2722,#2724,#1708,.T.);
#3307=EDGE_CURVE('',#2725,#2726,#1709,.T.);
#3308=EDGE_CURVE('',#2726,#2726,#2326,.T.);
#3309=EDGE_CURVE('',#2727,#2727,#2327,.T.);
#3310=EDGE_CURVE('',#2727,#2728,#1710,.T.);
#3311=EDGE_CURVE('',#2728,#2728,#2328,.T.);
#3312=EDGE_CURVE('',#2729,#2729,#2329,.T.);
#3313=EDGE_CURVE('',#2729,#2730,#1711,.T.);
#3314=EDGE_CURVE('',#2730,#2730,#2330,.T.);
#3315=EDGE_CURVE('',#2731,#2731,#2331,.T.);
#3316=EDGE_CURVE('',#2731,#2732,#1712,.T.);
#3317=EDGE_CURVE('',#2732,#2732,#2332,.T.);
#3318=EDGE_CURVE('',#2733,#2733,#2333,.T.);
#3319=EDGE_CURVE('',#2733,#2734,#1713,.T.);
#3320=EDGE_CURVE('',#2734,#2734,#2334,.T.);
#3321=EDGE_CURVE('',#2735,#2736,#1714,.T.);
#3322=EDGE_CURVE('',#2736,#2737,#1715,.T.);
#3323=EDGE_CURVE('',#2737,#2738,#1716,.T.);
#3324=EDGE_CURVE('',#2738,#2735,#1717,.T.);
#3325=EDGE_CURVE('',#2739,#2740,#1718,.T.);
#3326=EDGE_CURVE('',#2740,#2736,#2335,.T.);
#3327=EDGE_CURVE('',#2735,#2739,#2336,.T.);
#3328=EDGE_CURVE('',#2741,#2742,#1719,.T.);
#3329=EDGE_CURVE('',#2742,#2740,#1720,.T.);
#3330=EDGE_CURVE('',#2739,#2741,#1721,.T.);
#3331=EDGE_CURVE('',#2737,#2742,#2337,.T.);
#3332=EDGE_CURVE('',#2741,#2738,#2338,.T.);
#3333=EDGE_CURVE('',#2743,#2735,#1722,.T.);
#3334=EDGE_CURVE('',#2744,#2743,#2339,.T.);
#3335=EDGE_CURVE('',#2744,#2739,#1723,.T.);
#3336=EDGE_CURVE('',#2745,#2738,#1724,.T.);
#3337=EDGE_CURVE('',#2743,#2745,#1725,.T.);
#3338=EDGE_CURVE('',#2746,#2743,#1726,.T.);
#3339=EDGE_CURVE('',#2745,#2747,#1727,.T.);
#3340=EDGE_CURVE('',#2747,#2746,#1728,.T.);
#3341=EDGE_CURVE('',#2748,#2744,#1729,.T.);
#3342=EDGE_CURVE('',#2746,#2748,#2340,.T.);
#3343=EDGE_CURVE('',#2749,#2750,#1730,.T.);
#3344=EDGE_CURVE('',#2750,#2744,#1731,.T.);
#3345=EDGE_CURVE('',#2748,#2749,#1732,.T.);
#3346=EDGE_CURVE('',#2745,#2750,#2341,.T.);
#3347=EDGE_CURVE('',#2749,#2747,#2342,.T.);
#3348=EDGE_CURVE('',#2750,#2741,#1733,.T.);
#3349=EDGE_CURVE('',#2751,#2752,#1734,.T.);
#3350=EDGE_CURVE('',#2751,#2753,#1735,.T.);
#3351=EDGE_CURVE('',#2753,#2754,#1736,.T.);
#3352=EDGE_CURVE('',#2752,#2754,#1737,.T.);
#3353=EDGE_CURVE('',#2755,#2751,#1738,.T.);
#3354=EDGE_CURVE('',#2755,#2756,#1739,.T.);
#3355=EDGE_CURVE('',#2756,#2753,#1740,.T.);
#3356=EDGE_CURVE('',#2757,#2755,#1741,.T.);
#3357=EDGE_CURVE('',#2757,#2758,#1742,.T.);
#3358=EDGE_CURVE('',#2758,#2756,#1743,.T.);
#3359=EDGE_CURVE('',#2759,#2757,#1744,.T.);
#3360=EDGE_CURVE('',#2759,#2760,#1745,.T.);
#3361=EDGE_CURVE('',#2760,#2758,#1746,.T.);
#3362=EDGE_CURVE('',#2761,#2759,#1747,.T.);
#3363=EDGE_CURVE('',#2761,#2762,#1748,.T.);
#3364=EDGE_CURVE('',#2762,#2760,#1749,.T.);
#3365=EDGE_CURVE('',#2752,#2761,#1750,.T.);
#3366=EDGE_CURVE('',#2754,#2762,#1751,.T.);
#3367=EDGE_CURVE('',#2763,#2763,#2343,.T.);
#3368=EDGE_CURVE('',#2764,#2764,#2344,.T.);
#3369=EDGE_CURVE('',#2764,#2763,#1752,.T.);
#3370=EDGE_CURVE('',#2765,#2765,#2345,.F.);
#3371=EDGE_CURVE('',#2765,#2764,#1753,.T.);
#3372=EDGE_CURVE('',#2766,#2766,#2346,.T.);
#3373=EDGE_CURVE('',#2766,#2765,#1754,.T.);
#3374=EDGE_CURVE('',#2767,#2768,#1755,.T.);
#3375=EDGE_CURVE('',#2768,#2769,#1756,.T.);
#3376=EDGE_CURVE('',#2769,#2770,#1757,.T.);
#3377=EDGE_CURVE('',#2767,#2770,#1758,.T.);
#3378=EDGE_CURVE('',#2768,#2771,#1759,.T.);
#3379=EDGE_CURVE('',#2771,#2772,#1760,.T.);
#3380=EDGE_CURVE('',#2772,#2769,#1761,.T.);
#3381=EDGE_CURVE('',#2771,#2773,#1762,.T.);
#3382=EDGE_CURVE('',#2773,#2774,#1763,.T.);
#3383=EDGE_CURVE('',#2774,#2772,#1764,.T.);
#3384=EDGE_CURVE('',#2773,#2775,#1765,.T.);
#3385=EDGE_CURVE('',#2775,#2776,#1766,.T.);
#3386=EDGE_CURVE('',#2776,#2774,#1767,.T.);
#3387=EDGE_CURVE('',#2775,#2777,#1768,.T.);
#3388=EDGE_CURVE('',#2777,#2778,#1769,.T.);
#3389=EDGE_CURVE('',#2778,#2776,#1770,.T.);
#3390=EDGE_CURVE('',#2777,#2767,#1771,.T.);
#3391=EDGE_CURVE('',#2770,#2778,#1772,.T.);
#3392=EDGE_CURVE('',#2779,#2779,#2347,.T.);
#3393=EDGE_CURVE('',#2780,#2780,#2348,.T.);
#3394=EDGE_CURVE('',#2781,#2781,#2349,.T.);
#3395=EDGE_CURVE('',#2781,#2780,#1773,.T.);
#3396=EDGE_CURVE('',#2782,#2782,#2350,.T.);
#3397=EDGE_CURVE('',#2782,#2781,#1774,.T.);
#3398=EDGE_CURVE('',#2783,#2783,#2351,.T.);
#3399=EDGE_CURVE('',#2783,#2782,#1775,.T.);
#3400=EDGE_CURVE('',#2784,#2784,#2352,.T.);
#3401=EDGE_CURVE('',#2785,#2785,#2353,.F.);
#3402=EDGE_CURVE('',#2785,#2784,#1776,.T.);
#3403=EDGE_CURVE('',#2779,#2785,#1777,.T.);
#3404=EDGE_CURVE('',#2786,#2787,#2354,.T.);
#3405=EDGE_CURVE('',#2787,#2786,#2355,.T.);
#3406=EDGE_CURVE('',#2787,#2788,#2356,.T.);
#3407=EDGE_CURVE('',#2789,#2788,#2357,.T.);
#3408=EDGE_CURVE('',#2788,#2789,#2358,.T.);
#3409=EDGE_CURVE('',#2789,#2790,#1778,.T.);
#3410=EDGE_CURVE('',#2790,#2790,#2359,.T.);
#3411=EDGE_CURVE('',#2791,#2791,#2360,.T.);
#3412=EDGE_CURVE('',#2791,#2792,#1779,.T.);
#3413=EDGE_CURVE('',#2792,#2792,#2361,.T.);
#3414=EDGE_CURVE('',#2792,#2793,#1780,.T.);
#3415=EDGE_CURVE('',#2793,#2793,#2362,.T.);
#3416=EDGE_CURVE('',#2794,#2794,#2363,.T.);
#3417=EDGE_CURVE('',#2794,#2786,#1781,.T.);
#3418=EDGE_CURVE('',#2795,#2795,#2364,.T.);
#3419=EDGE_CURVE('',#2795,#2791,#1782,.T.);
#3420=EDGE_CURVE('',#2796,#2797,#2365,.T.);
#3421=EDGE_CURVE('',#2797,#2796,#2366,.T.);
#3422=EDGE_CURVE('',#2797,#2798,#2367,.T.);
#3423=EDGE_CURVE('',#2799,#2798,#2368,.T.);
#3424=EDGE_CURVE('',#2798,#2799,#2369,.T.);
#3425=EDGE_CURVE('',#2800,#2800,#2370,.T.);
#3426=EDGE_CURVE('',#2800,#2799,#1783,.T.);
#3427=EDGE_CURVE('',#2801,#2801,#2371,.T.);
#3428=EDGE_CURVE('',#2802,#2802,#2372,.T.);
#3429=EDGE_CURVE('',#2803,#2803,#2373,.T.);
#3430=EDGE_CURVE('',#2803,#2801,#1784,.T.);
#3431=EDGE_CURVE('',#2804,#2804,#2374,.T.);
#3432=EDGE_CURVE('',#2804,#2803,#1785,.T.);
#3433=EDGE_CURVE('',#2805,#2805,#2375,.T.);
#3434=EDGE_CURVE('',#2805,#2804,#1786,.T.);
#3435=EDGE_CURVE('',#2796,#2802,#1787,.T.);
#3436=EDGE_CURVE('',#2806,#2807,#2376,.T.);
#3437=EDGE_CURVE('',#2808,#2809,#2377,.T.);
#3438=EDGE_CURVE('',#2810,#2811,#2378,.T.);
#3439=EDGE_CURVE('',#2812,#2813,#2379,.T.);
#3440=EDGE_CURVE('',#2814,#2815,#2380,.T.);
#3441=EDGE_CURVE('',#2816,#2817,#2381,.T.);
#3442=EDGE_CURVE('',#2818,#2819,#2382,.T.);
#3443=EDGE_CURVE('',#2820,#2821,#2383,.T.);
#3444=EDGE_CURVE('',#2822,#2823,#249,.T.);
#3445=EDGE_CURVE('',#2824,#2822,#2384,.T.);
#3446=EDGE_CURVE('',#2825,#2824,#250,.T.);
#3447=EDGE_CURVE('',#2823,#2825,#2385,.T.);
#3448=EDGE_CURVE('',#2826,#2824,#2386,.T.);
#3449=EDGE_CURVE('',#2826,#2827,#251,.T.);
#3450=EDGE_CURVE('',#2828,#2827,#2387,.T.);
#3451=EDGE_CURVE('',#2828,#2829,#252,.T.);
#3452=EDGE_CURVE('',#2830,#2829,#2388,.T.);
#3453=EDGE_CURVE('',#2830,#2831,#253,.T.);
#3454=EDGE_CURVE('',#2831,#2832,#1788,.T.);
#3455=EDGE_CURVE('',#2832,#2832,#2389,.T.);
#3456=EDGE_CURVE('',#2831,#2833,#254,.T.);
#3457=EDGE_CURVE('',#2834,#2833,#2390,.T.);
#3458=EDGE_CURVE('',#2834,#2835,#255,.T.);
#3459=EDGE_CURVE('',#2836,#2835,#2391,.T.);
#3460=EDGE_CURVE('',#2836,#2837,#256,.T.);
#3461=EDGE_CURVE('',#2838,#2837,#2392,.T.);
#3462=EDGE_CURVE('',#2838,#2839,#257,.T.);
#3463=EDGE_CURVE('',#2840,#2839,#2393,.T.);
#3464=EDGE_CURVE('',#2840,#2841,#258,.T.);
#3465=EDGE_CURVE('',#2825,#2841,#2394,.T.);
#3466=EDGE_CURVE('',#2822,#2842,#2395,.T.);
#3467=EDGE_CURVE('',#2842,#2826,#2396,.T.);
#3468=EDGE_CURVE('',#2843,#2842,#259,.T.);
#3469=EDGE_CURVE('',#2827,#2843,#2397,.T.);
#3470=EDGE_CURVE('',#2843,#2844,#2398,.T.);
#3471=EDGE_CURVE('',#2844,#2828,#2399,.T.);
#3472=EDGE_CURVE('',#2845,#2844,#260,.T.);
#3473=EDGE_CURVE('',#2829,#2845,#2400,.T.);
#3474=EDGE_CURVE('',#2845,#2846,#2401,.T.);
#3475=EDGE_CURVE('',#2846,#2830,#2402,.T.);
#3476=EDGE_CURVE('',#2847,#2848,#261,.T.);
#3477=EDGE_CURVE('',#2833,#2847,#2403,.T.);
#3478=EDGE_CURVE('',#2848,#2846,#262,.T.);
#3479=EDGE_CURVE('',#2847,#2849,#2404,.T.);
#3480=EDGE_CURVE('',#2849,#2834,#2405,.T.);
#3481=EDGE_CURVE('',#2850,#2849,#263,.T.);
#3482=EDGE_CURVE('',#2835,#2850,#2406,.T.);
#3483=EDGE_CURVE('',#2850,#2851,#2407,.T.);
#3484=EDGE_CURVE('',#2851,#2836,#2408,.T.);
#3485=EDGE_CURVE('',#2852,#2851,#264,.T.);
#3486=EDGE_CURVE('',#2837,#2852,#2409,.T.);
#3487=EDGE_CURVE('',#2852,#2853,#2410,.T.);
#3488=EDGE_CURVE('',#2853,#2838,#2411,.T.);
#3489=EDGE_CURVE('',#2854,#2853,#265,.T.);
#3490=EDGE_CURVE('',#2839,#2854,#2412,.T.);
#3491=EDGE_CURVE('',#2855,#2855,#2413,.T.);
#3492=EDGE_CURVE('',#2855,#2848,#1789,.T.);
#3493=EDGE_CURVE('',#2856,#2823,#2414,.T.);
#3494=EDGE_CURVE('',#2856,#2857,#266,.T.);
#3495=EDGE_CURVE('',#2854,#2857,#2415,.T.);
#3496=EDGE_CURVE('',#2841,#2856,#2416,.T.);
#3497=EDGE_CURVE('',#2857,#2840,#2417,.T.);
#3498=EDGE_CURVE('',#2858,#2858,#2418,.T.);
#3499=EDGE_CURVE('',#2859,#2859,#2419,.T.);
#3500=EDGE_CURVE('',#2860,#2860,#2420,.T.);
#3501=EDGE_CURVE('',#2860,#2858,#1790,.T.);
#3502=EDGE_CURVE('',#2861,#2861,#2421,.T.);
#3503=EDGE_CURVE('',#2861,#2859,#1791,.T.);
#3504=EDGE_CURVE('',#2862,#2862,#2422,.T.);
#3505=EDGE_CURVE('',#2863,#2863,#2423,.T.);
#3506=EDGE_CURVE('',#2864,#2864,#2424,.T.);
#3507=EDGE_CURVE('',#2864,#2862,#1792,.T.);
#3508=EDGE_CURVE('',#2865,#2865,#2425,.T.);
#3509=EDGE_CURVE('',#2865,#2863,#1793,.T.);
#3510=EDGE_CURVE('',#2866,#2866,#2426,.T.);
#3511=EDGE_CURVE('',#2867,#2867,#2427,.T.);
#3512=EDGE_CURVE('',#2867,#2866,#1794,.T.);
#3513=EDGE_CURVE('',#2868,#2868,#2428,.T.);
#3514=EDGE_CURVE('',#2868,#2867,#1795,.T.);
#3515=EDGE_CURVE('',#2869,#2869,#2429,.T.);
#3516=EDGE_CURVE('',#2869,#2868,#1796,.T.);
#3517=EDGE_CURVE('',#2870,#2870,#2430,.T.);
#3518=EDGE_CURVE('',#2871,#2871,#2431,.F.);
#3519=EDGE_CURVE('',#2871,#2870,#1797,.T.);
#3520=EDGE_CURVE('',#2872,#2872,#2432,.F.);
#3521=EDGE_CURVE('',#2872,#2871,#1798,.T.);
#3522=EDGE_CURVE('',#2873,#2873,#2433,.T.);
#3523=EDGE_CURVE('',#2873,#2872,#1799,.T.);
#3524=EDGE_CURVE('',#2874,#2875,#1800,.T.);
#3525=EDGE_CURVE('',#2875,#2876,#1801,.T.);
#3526=EDGE_CURVE('',#2876,#2877,#1802,.T.);
#3527=EDGE_CURVE('',#2874,#2877,#1803,.T.);
#3528=EDGE_CURVE('',#2875,#2878,#1804,.T.);
#3529=EDGE_CURVE('',#2878,#2879,#1805,.T.);
#3530=EDGE_CURVE('',#2879,#2876,#1806,.T.);
#3531=EDGE_CURVE('',#2878,#2880,#1807,.T.);
#3532=EDGE_CURVE('',#2880,#2881,#1808,.T.);
#3533=EDGE_CURVE('',#2881,#2879,#1809,.T.);
#3534=EDGE_CURVE('',#2880,#2882,#1810,.T.);
#3535=EDGE_CURVE('',#2882,#2883,#1811,.T.);
#3536=EDGE_CURVE('',#2883,#2881,#1812,.T.);
#3537=EDGE_CURVE('',#2882,#2884,#1813,.T.);
#3538=EDGE_CURVE('',#2884,#2885,#1814,.T.);
#3539=EDGE_CURVE('',#2885,#2883,#1815,.T.);
#3540=EDGE_CURVE('',#2884,#2874,#1816,.T.);
#3541=EDGE_CURVE('',#2877,#2885,#1817,.T.);
#3542=EDGE_CURVE('',#2886,#2886,#2434,.T.);
#3543=EDGE_CURVE('',#2886,#2887,#1818,.T.);
#3544=EDGE_CURVE('',#2887,#2887,#2435,.T.);
#3545=EDGE_CURVE('',#2888,#2888,#2436,.T.);
#3546=EDGE_CURVE('',#2888,#2889,#1819,.T.);
#3547=EDGE_CURVE('',#2889,#2889,#2437,.T.);
#3548=EDGE_CURVE('',#2890,#2890,#2438,.T.);
#3549=EDGE_CURVE('',#2890,#2891,#1820,.T.);
#3550=EDGE_CURVE('',#2891,#2891,#2439,.T.);
#3551=EDGE_CURVE('',#2892,#2892,#2440,.T.);
#3552=EDGE_CURVE('',#2892,#2893,#1821,.T.);
#3553=EDGE_CURVE('',#2893,#2893,#2441,.T.);
#3554=EDGE_CURVE('',#2894,#2894,#2442,.T.);
#3555=EDGE_CURVE('',#2894,#2895,#1822,.T.);
#3556=EDGE_CURVE('',#2895,#2895,#2443,.T.);
#3557=ORIENTED_EDGE('',*,*,#2896,.F.);
#3558=ORIENTED_EDGE('',*,*,#2897,.T.);
#3559=ORIENTED_EDGE('',*,*,#2898,.F.);
#3560=ORIENTED_EDGE('',*,*,#2897,.F.);
#3561=ORIENTED_EDGE('',*,*,#2899,.F.);
#3562=ORIENTED_EDGE('',*,*,#2900,.T.);
#3563=ORIENTED_EDGE('',*,*,#2901,.F.);
#3564=ORIENTED_EDGE('',*,*,#2900,.F.);
#3565=ORIENTED_EDGE('',*,*,#2902,.F.);
#3566=ORIENTED_EDGE('',*,*,#2903,.T.);
#3567=ORIENTED_EDGE('',*,*,#2904,.F.);
#3568=ORIENTED_EDGE('',*,*,#2903,.F.);
#3569=ORIENTED_EDGE('',*,*,#2905,.F.);
#3570=ORIENTED_EDGE('',*,*,#2906,.T.);
#3571=ORIENTED_EDGE('',*,*,#2907,.F.);
#3572=ORIENTED_EDGE('',*,*,#2906,.F.);
#3573=ORIENTED_EDGE('',*,*,#2908,.T.);
#3574=ORIENTED_EDGE('',*,*,#2909,.T.);
#3575=ORIENTED_EDGE('',*,*,#2910,.F.);
#3576=ORIENTED_EDGE('',*,*,#2911,.F.);
#3577=ORIENTED_EDGE('',*,*,#2912,.T.);
#3578=ORIENTED_EDGE('',*,*,#2911,.T.);
#3579=ORIENTED_EDGE('',*,*,#2913,.F.);
#3580=ORIENTED_EDGE('',*,*,#2914,.F.);
#3581=ORIENTED_EDGE('',*,*,#2915,.T.);
#3582=ORIENTED_EDGE('',*,*,#2914,.T.);
#3583=ORIENTED_EDGE('',*,*,#2916,.F.);
#3584=ORIENTED_EDGE('',*,*,#2917,.F.);
#3585=ORIENTED_EDGE('',*,*,#2918,.T.);
#3586=ORIENTED_EDGE('',*,*,#2917,.T.);
#3587=ORIENTED_EDGE('',*,*,#2919,.F.);
#3588=ORIENTED_EDGE('',*,*,#2909,.F.);
#3589=ORIENTED_EDGE('',*,*,#2919,.T.);
#3590=ORIENTED_EDGE('',*,*,#2916,.T.);
#3591=ORIENTED_EDGE('',*,*,#2913,.T.);
#3592=ORIENTED_EDGE('',*,*,#2910,.T.);
#3593=ORIENTED_EDGE('',*,*,#2898,.T.);
#3594=ORIENTED_EDGE('',*,*,#2901,.T.);
#3595=ORIENTED_EDGE('',*,*,#2904,.T.);
#3596=ORIENTED_EDGE('',*,*,#2907,.T.);
#3597=ORIENTED_EDGE('',*,*,#2918,.F.);
#3598=ORIENTED_EDGE('',*,*,#2908,.F.);
#3599=ORIENTED_EDGE('',*,*,#2912,.F.);
#3600=ORIENTED_EDGE('',*,*,#2915,.F.);
#3601=ORIENTED_EDGE('',*,*,#2896,.T.);
#3602=ORIENTED_EDGE('',*,*,#2899,.T.);
#3603=ORIENTED_EDGE('',*,*,#2902,.T.);
#3604=ORIENTED_EDGE('',*,*,#2905,.T.);
#3605=ORIENTED_EDGE('',*,*,#2920,.T.);
#3606=ORIENTED_EDGE('',*,*,#2921,.T.);
#3607=ORIENTED_EDGE('',*,*,#2922,.F.);
#3608=ORIENTED_EDGE('',*,*,#2923,.F.);
#3609=ORIENTED_EDGE('',*,*,#2924,.T.);
#3610=ORIENTED_EDGE('',*,*,#2923,.T.);
#3611=ORIENTED_EDGE('',*,*,#2925,.F.);
#3612=ORIENTED_EDGE('',*,*,#2926,.F.);
#3613=ORIENTED_EDGE('',*,*,#2927,.T.);
#3614=ORIENTED_EDGE('',*,*,#2926,.T.);
#3615=ORIENTED_EDGE('',*,*,#2928,.F.);
#3616=ORIENTED_EDGE('',*,*,#2929,.F.);
#3617=ORIENTED_EDGE('',*,*,#2930,.T.);
#3618=ORIENTED_EDGE('',*,*,#2929,.T.);
#3619=ORIENTED_EDGE('',*,*,#2931,.F.);
#3620=ORIENTED_EDGE('',*,*,#2921,.F.);
#3621=ORIENTED_EDGE('',*,*,#2931,.T.);
#3622=ORIENTED_EDGE('',*,*,#2928,.T.);
#3623=ORIENTED_EDGE('',*,*,#2925,.T.);
#3624=ORIENTED_EDGE('',*,*,#2922,.T.);
#3625=ORIENTED_EDGE('',*,*,#2930,.F.);
#3626=ORIENTED_EDGE('',*,*,#2920,.F.);
#3627=ORIENTED_EDGE('',*,*,#2924,.F.);
#3628=ORIENTED_EDGE('',*,*,#2927,.F.);
#3629=ORIENTED_EDGE('',*,*,#2932,.T.);
#3630=ORIENTED_EDGE('',*,*,#2933,.T.);
#3631=ORIENTED_EDGE('',*,*,#2934,.F.);
#3632=ORIENTED_EDGE('',*,*,#2935,.F.);
#3633=ORIENTED_EDGE('',*,*,#2936,.T.);
#3634=ORIENTED_EDGE('',*,*,#2935,.T.);
#3635=ORIENTED_EDGE('',*,*,#2937,.F.);
#3636=ORIENTED_EDGE('',*,*,#2938,.F.);
#3637=ORIENTED_EDGE('',*,*,#2939,.T.);
#3638=ORIENTED_EDGE('',*,*,#2938,.T.);
#3639=ORIENTED_EDGE('',*,*,#2940,.F.);
#3640=ORIENTED_EDGE('',*,*,#2941,.F.);
#3641=ORIENTED_EDGE('',*,*,#2942,.T.);
#3642=ORIENTED_EDGE('',*,*,#2941,.T.);
#3643=ORIENTED_EDGE('',*,*,#2943,.F.);
#3644=ORIENTED_EDGE('',*,*,#2933,.F.);
#3645=ORIENTED_EDGE('',*,*,#2943,.T.);
#3646=ORIENTED_EDGE('',*,*,#2940,.T.);
#3647=ORIENTED_EDGE('',*,*,#2937,.T.);
#3648=ORIENTED_EDGE('',*,*,#2934,.T.);
#3649=ORIENTED_EDGE('',*,*,#2942,.F.);
#3650=ORIENTED_EDGE('',*,*,#2932,.F.);
#3651=ORIENTED_EDGE('',*,*,#2936,.F.);
#3652=ORIENTED_EDGE('',*,*,#2939,.F.);
#3653=ORIENTED_EDGE('',*,*,#2944,.F.);
#3654=ORIENTED_EDGE('',*,*,#2945,.T.);
#3655=ORIENTED_EDGE('',*,*,#2946,.F.);
#3656=ORIENTED_EDGE('',*,*,#2945,.F.);
#3657=ORIENTED_EDGE('',*,*,#2947,.F.);
#3658=ORIENTED_EDGE('',*,*,#2948,.T.);
#3659=ORIENTED_EDGE('',*,*,#2949,.F.);
#3660=ORIENTED_EDGE('',*,*,#2948,.F.);
#3661=ORIENTED_EDGE('',*,*,#2950,.F.);
#3662=ORIENTED_EDGE('',*,*,#2951,.T.);
#3663=ORIENTED_EDGE('',*,*,#2952,.F.);
#3664=ORIENTED_EDGE('',*,*,#2951,.F.);
#3665=ORIENTED_EDGE('',*,*,#2953,.F.);
#3666=ORIENTED_EDGE('',*,*,#2954,.T.);
#3667=ORIENTED_EDGE('',*,*,#2955,.F.);
#3668=ORIENTED_EDGE('',*,*,#2954,.F.);
#3669=ORIENTED_EDGE('',*,*,#2956,.F.);
#3670=ORIENTED_EDGE('',*,*,#2957,.T.);
#3671=ORIENTED_EDGE('',*,*,#2958,.F.);
#3672=ORIENTED_EDGE('',*,*,#2957,.F.);
#3673=ORIENTED_EDGE('',*,*,#2959,.F.);
#3674=ORIENTED_EDGE('',*,*,#2960,.T.);
#3675=ORIENTED_EDGE('',*,*,#2961,.F.);
#3676=ORIENTED_EDGE('',*,*,#2960,.F.);
#3677=ORIENTED_EDGE('',*,*,#2962,.F.);
#3678=ORIENTED_EDGE('',*,*,#2963,.T.);
#3679=ORIENTED_EDGE('',*,*,#2964,.F.);
#3680=ORIENTED_EDGE('',*,*,#2963,.F.);
#3681=ORIENTED_EDGE('',*,*,#2965,.F.);
#3682=ORIENTED_EDGE('',*,*,#2966,.T.);
#3683=ORIENTED_EDGE('',*,*,#2967,.F.);
#3684=ORIENTED_EDGE('',*,*,#2966,.F.);
#3685=ORIENTED_EDGE('',*,*,#2968,.F.);
#3686=ORIENTED_EDGE('',*,*,#2969,.T.);
#3687=ORIENTED_EDGE('',*,*,#2970,.F.);
#3688=ORIENTED_EDGE('',*,*,#2969,.F.);
#3689=ORIENTED_EDGE('',*,*,#2971,.F.);
#3690=ORIENTED_EDGE('',*,*,#2972,.F.);
#3691=ORIENTED_EDGE('',*,*,#2973,.T.);
#3692=ORIENTED_EDGE('',*,*,#2974,.F.);
#3693=ORIENTED_EDGE('',*,*,#2958,.T.);
#3694=ORIENTED_EDGE('',*,*,#2967,.T.);
#3695=ORIENTED_EDGE('',*,*,#2975,.F.);
#3696=ORIENTED_EDGE('',*,*,#2976,.F.);
#3697=ORIENTED_EDGE('',*,*,#2977,.F.);
#3698=ORIENTED_EDGE('',*,*,#2978,.F.);
#3699=ORIENTED_EDGE('',*,*,#2961,.T.);
#3700=ORIENTED_EDGE('',*,*,#2964,.T.);
#3701=ORIENTED_EDGE('',*,*,#2979,.F.);
#3702=ORIENTED_EDGE('',*,*,#2977,.T.);
#3703=ORIENTED_EDGE('',*,*,#2980,.F.);
#3704=ORIENTED_EDGE('',*,*,#2981,.F.);
#3705=ORIENTED_EDGE('',*,*,#2982,.F.);
#3706=ORIENTED_EDGE('',*,*,#2983,.T.);
#3707=ORIENTED_EDGE('',*,*,#2984,.F.);
#3708=ORIENTED_EDGE('',*,*,#2973,.F.);
#3709=ORIENTED_EDGE('',*,*,#2985,.T.);
#3710=ORIENTED_EDGE('',*,*,#2986,.F.);
#3711=ORIENTED_EDGE('',*,*,#2987,.F.);
#3712=ORIENTED_EDGE('',*,*,#2978,.T.);
#3713=ORIENTED_EDGE('',*,*,#2979,.T.);
#3714=ORIENTED_EDGE('',*,*,#2988,.T.);
#3715=ORIENTED_EDGE('',*,*,#2982,.T.);
#3716=ORIENTED_EDGE('',*,*,#2972,.T.);
#3717=ORIENTED_EDGE('',*,*,#2968,.T.);
#3718=ORIENTED_EDGE('',*,*,#2953,.T.);
#3719=ORIENTED_EDGE('',*,*,#2950,.T.);
#3720=ORIENTED_EDGE('',*,*,#2947,.T.);
#3721=ORIENTED_EDGE('',*,*,#2944,.T.);
#3722=ORIENTED_EDGE('',*,*,#2971,.T.);
#3723=ORIENTED_EDGE('',*,*,#2989,.T.);
#3724=ORIENTED_EDGE('',*,*,#2990,.F.);
#3725=ORIENTED_EDGE('',*,*,#2985,.F.);
#3726=ORIENTED_EDGE('',*,*,#2991,.T.);
#3727=ORIENTED_EDGE('',*,*,#2992,.F.);
#3728=ORIENTED_EDGE('',*,*,#2989,.F.);
#3729=ORIENTED_EDGE('',*,*,#2974,.T.);
#3730=ORIENTED_EDGE('',*,*,#2984,.T.);
#3731=ORIENTED_EDGE('',*,*,#2993,.T.);
#3732=ORIENTED_EDGE('',*,*,#2980,.T.);
#3733=ORIENTED_EDGE('',*,*,#2976,.T.);
#3734=ORIENTED_EDGE('',*,*,#2970,.T.);
#3735=ORIENTED_EDGE('',*,*,#2955,.T.);
#3736=ORIENTED_EDGE('',*,*,#2952,.T.);
#3737=ORIENTED_EDGE('',*,*,#2949,.T.);
#3738=ORIENTED_EDGE('',*,*,#2946,.T.);
#3739=ORIENTED_EDGE('',*,*,#2975,.T.);
#3740=ORIENTED_EDGE('',*,*,#2987,.T.);
#3741=ORIENTED_EDGE('',*,*,#2994,.F.);
#3742=ORIENTED_EDGE('',*,*,#2991,.F.);
#3743=ORIENTED_EDGE('',*,*,#2994,.T.);
#3744=ORIENTED_EDGE('',*,*,#2986,.T.);
#3745=ORIENTED_EDGE('',*,*,#2990,.T.);
#3746=ORIENTED_EDGE('',*,*,#2992,.T.);
#3747=ORIENTED_EDGE('',*,*,#2993,.F.);
#3748=ORIENTED_EDGE('',*,*,#2983,.F.);
#3749=ORIENTED_EDGE('',*,*,#2988,.F.);
#3750=ORIENTED_EDGE('',*,*,#2981,.T.);
#3751=ORIENTED_EDGE('',*,*,#2956,.T.);
#3752=ORIENTED_EDGE('',*,*,#2959,.T.);
#3753=ORIENTED_EDGE('',*,*,#2962,.T.);
#3754=ORIENTED_EDGE('',*,*,#2965,.T.);
#3755=ORIENTED_EDGE('',*,*,#2995,.F.);
#3756=ORIENTED_EDGE('',*,*,#2996,.T.);
#3757=ORIENTED_EDGE('',*,*,#2997,.T.);
#3758=ORIENTED_EDGE('',*,*,#2996,.F.);
#3759=ORIENTED_EDGE('',*,*,#2998,.F.);
#3760=ORIENTED_EDGE('',*,*,#2999,.T.);
#3761=ORIENTED_EDGE('',*,*,#3000,.T.);
#3762=ORIENTED_EDGE('',*,*,#2999,.F.);
#3763=ORIENTED_EDGE('',*,*,#2998,.T.);
#3764=ORIENTED_EDGE('',*,*,#2995,.T.);
#3765=ORIENTED_EDGE('',*,*,#3000,.F.);
#3766=ORIENTED_EDGE('',*,*,#2997,.F.);
#3767=ORIENTED_EDGE('',*,*,#3001,.F.);
#3768=ORIENTED_EDGE('',*,*,#3002,.T.);
#3769=ORIENTED_EDGE('',*,*,#3003,.F.);
#3770=ORIENTED_EDGE('',*,*,#3002,.F.);
#3771=ORIENTED_EDGE('',*,*,#3004,.F.);
#3772=ORIENTED_EDGE('',*,*,#3005,.T.);
#3773=ORIENTED_EDGE('',*,*,#3006,.F.);
#3774=ORIENTED_EDGE('',*,*,#3005,.F.);
#3775=ORIENTED_EDGE('',*,*,#3007,.F.);
#3776=ORIENTED_EDGE('',*,*,#3008,.T.);
#3777=ORIENTED_EDGE('',*,*,#3009,.F.);
#3778=ORIENTED_EDGE('',*,*,#3008,.F.);
#3779=ORIENTED_EDGE('',*,*,#3010,.F.);
#3780=ORIENTED_EDGE('',*,*,#3011,.T.);
#3781=ORIENTED_EDGE('',*,*,#3012,.F.);
#3782=ORIENTED_EDGE('',*,*,#3011,.F.);
#3783=ORIENTED_EDGE('',*,*,#3013,.F.);
#3784=ORIENTED_EDGE('',*,*,#3014,.T.);
#3785=ORIENTED_EDGE('',*,*,#3015,.F.);
#3786=ORIENTED_EDGE('',*,*,#3014,.F.);
#3787=ORIENTED_EDGE('',*,*,#3013,.T.);
#3788=ORIENTED_EDGE('',*,*,#3016,.T.);
#3789=ORIENTED_EDGE('',*,*,#3016,.F.);
#3790=ORIENTED_EDGE('',*,*,#3017,.T.);
#3791=ORIENTED_EDGE('',*,*,#3018,.T.);
#3792=ORIENTED_EDGE('',*,*,#3017,.F.);
#3793=ORIENTED_EDGE('',*,*,#3019,.F.);
#3794=ORIENTED_EDGE('',*,*,#3020,.T.);
#3795=ORIENTED_EDGE('',*,*,#3021,.T.);
#3796=ORIENTED_EDGE('',*,*,#3020,.F.);
#3797=ORIENTED_EDGE('',*,*,#3019,.T.);
#3798=ORIENTED_EDGE('',*,*,#3015,.T.);
#3799=ORIENTED_EDGE('',*,*,#3012,.T.);
#3800=ORIENTED_EDGE('',*,*,#3009,.T.);
#3801=ORIENTED_EDGE('',*,*,#3006,.T.);
#3802=ORIENTED_EDGE('',*,*,#3003,.T.);
#3803=ORIENTED_EDGE('',*,*,#3021,.F.);
#3804=ORIENTED_EDGE('',*,*,#3018,.F.);
#3805=ORIENTED_EDGE('',*,*,#3010,.T.);
#3806=ORIENTED_EDGE('',*,*,#3007,.T.);
#3807=ORIENTED_EDGE('',*,*,#3004,.T.);
#3808=ORIENTED_EDGE('',*,*,#3001,.T.);
#3809=ORIENTED_EDGE('',*,*,#3022,.F.);
#3810=ORIENTED_EDGE('',*,*,#3023,.T.);
#3811=ORIENTED_EDGE('',*,*,#3024,.F.);
#3812=ORIENTED_EDGE('',*,*,#3023,.F.);
#3813=ORIENTED_EDGE('',*,*,#3025,.F.);
#3814=ORIENTED_EDGE('',*,*,#3026,.T.);
#3815=ORIENTED_EDGE('',*,*,#3027,.F.);
#3816=ORIENTED_EDGE('',*,*,#3026,.F.);
#3817=ORIENTED_EDGE('',*,*,#3028,.F.);
#3818=ORIENTED_EDGE('',*,*,#3029,.T.);
#3819=ORIENTED_EDGE('',*,*,#3030,.F.);
#3820=ORIENTED_EDGE('',*,*,#3029,.F.);
#3821=ORIENTED_EDGE('',*,*,#3031,.F.);
#3822=ORIENTED_EDGE('',*,*,#3032,.T.);
#3823=ORIENTED_EDGE('',*,*,#3033,.F.);
#3824=ORIENTED_EDGE('',*,*,#3032,.F.);
#3825=ORIENTED_EDGE('',*,*,#3034,.F.);
#3826=ORIENTED_EDGE('',*,*,#3035,.T.);
#3827=ORIENTED_EDGE('',*,*,#3036,.T.);
#3828=ORIENTED_EDGE('',*,*,#3035,.F.);
#3829=ORIENTED_EDGE('',*,*,#3036,.F.);
#3830=ORIENTED_EDGE('',*,*,#3037,.F.);
#3831=ORIENTED_EDGE('',*,*,#3038,.F.);
#3832=ORIENTED_EDGE('',*,*,#3039,.T.);
#3833=ORIENTED_EDGE('',*,*,#3037,.T.);
#3834=ORIENTED_EDGE('',*,*,#3039,.F.);
#3835=ORIENTED_EDGE('',*,*,#3040,.F.);
#3836=ORIENTED_EDGE('',*,*,#3041,.T.);
#3837=ORIENTED_EDGE('',*,*,#3042,.T.);
#3838=ORIENTED_EDGE('',*,*,#3041,.F.);
#3839=ORIENTED_EDGE('',*,*,#3040,.T.);
#3840=ORIENTED_EDGE('',*,*,#3038,.T.);
#3841=ORIENTED_EDGE('',*,*,#3033,.T.);
#3842=ORIENTED_EDGE('',*,*,#3030,.T.);
#3843=ORIENTED_EDGE('',*,*,#3027,.T.);
#3844=ORIENTED_EDGE('',*,*,#3024,.T.);
#3845=ORIENTED_EDGE('',*,*,#3042,.F.);
#3846=ORIENTED_EDGE('',*,*,#3034,.T.);
#3847=ORIENTED_EDGE('',*,*,#3031,.T.);
#3848=ORIENTED_EDGE('',*,*,#3028,.T.);
#3849=ORIENTED_EDGE('',*,*,#3025,.T.);
#3850=ORIENTED_EDGE('',*,*,#3022,.T.);
#3851=ORIENTED_EDGE('',*,*,#3043,.F.);
#3852=ORIENTED_EDGE('',*,*,#3044,.T.);
#3853=ORIENTED_EDGE('',*,*,#3045,.T.);
#3854=ORIENTED_EDGE('',*,*,#3044,.F.);
#3855=ORIENTED_EDGE('',*,*,#3046,.F.);
#3856=ORIENTED_EDGE('',*,*,#3047,.T.);
#3857=ORIENTED_EDGE('',*,*,#3048,.T.);
#3858=ORIENTED_EDGE('',*,*,#3047,.F.);
#3859=ORIENTED_EDGE('',*,*,#3046,.T.);
#3860=ORIENTED_EDGE('',*,*,#3043,.T.);
#3861=ORIENTED_EDGE('',*,*,#3048,.F.);
#3862=ORIENTED_EDGE('',*,*,#3045,.F.);
#3863=ORIENTED_EDGE('',*,*,#3049,.T.);
#3864=ORIENTED_EDGE('',*,*,#3050,.T.);
#3865=ORIENTED_EDGE('',*,*,#3051,.T.);
#3866=ORIENTED_EDGE('',*,*,#3052,.F.);
#3867=ORIENTED_EDGE('',*,*,#3053,.T.);
#3868=ORIENTED_EDGE('',*,*,#3054,.T.);
#3869=ORIENTED_EDGE('',*,*,#3055,.T.);
#3870=ORIENTED_EDGE('',*,*,#3050,.F.);
#3871=ORIENTED_EDGE('',*,*,#3056,.T.);
#3872=ORIENTED_EDGE('',*,*,#3057,.T.);
#3873=ORIENTED_EDGE('',*,*,#3058,.T.);
#3874=ORIENTED_EDGE('',*,*,#3054,.F.);
#3875=ORIENTED_EDGE('',*,*,#3059,.T.);
#3876=ORIENTED_EDGE('',*,*,#3060,.T.);
#3877=ORIENTED_EDGE('',*,*,#3061,.T.);
#3878=ORIENTED_EDGE('',*,*,#3057,.F.);
#3879=ORIENTED_EDGE('',*,*,#3062,.T.);
#3880=ORIENTED_EDGE('',*,*,#3063,.T.);
#3881=ORIENTED_EDGE('',*,*,#3064,.T.);
#3882=ORIENTED_EDGE('',*,*,#3060,.F.);
#3883=ORIENTED_EDGE('',*,*,#3065,.T.);
#3884=ORIENTED_EDGE('',*,*,#3052,.T.);
#3885=ORIENTED_EDGE('',*,*,#3066,.T.);
#3886=ORIENTED_EDGE('',*,*,#3063,.F.);
#3887=ORIENTED_EDGE('',*,*,#3065,.F.);
#3888=ORIENTED_EDGE('',*,*,#3062,.F.);
#3889=ORIENTED_EDGE('',*,*,#3059,.F.);
#3890=ORIENTED_EDGE('',*,*,#3056,.F.);
#3891=ORIENTED_EDGE('',*,*,#3053,.F.);
#3892=ORIENTED_EDGE('',*,*,#3049,.F.);
#3893=ORIENTED_EDGE('',*,*,#3066,.F.);
#3894=ORIENTED_EDGE('',*,*,#3051,.F.);
#3895=ORIENTED_EDGE('',*,*,#3055,.F.);
#3896=ORIENTED_EDGE('',*,*,#3058,.F.);
#3897=ORIENTED_EDGE('',*,*,#3061,.F.);
#3898=ORIENTED_EDGE('',*,*,#3064,.F.);
#3899=ORIENTED_EDGE('',*,*,#3067,.F.);
#3900=ORIENTED_EDGE('',*,*,#3068,.F.);
#3901=ORIENTED_EDGE('',*,*,#3069,.F.);
#3902=ORIENTED_EDGE('',*,*,#3070,.T.);
#3903=ORIENTED_EDGE('',*,*,#3068,.T.);
#3904=ORIENTED_EDGE('',*,*,#3070,.F.);
#3905=ORIENTED_EDGE('',*,*,#3071,.F.);
#3906=ORIENTED_EDGE('',*,*,#3072,.T.);
#3907=ORIENTED_EDGE('',*,*,#3069,.T.);
#3908=ORIENTED_EDGE('',*,*,#3072,.F.);
#3909=ORIENTED_EDGE('',*,*,#3073,.F.);
#3910=ORIENTED_EDGE('',*,*,#3074,.T.);
#3911=ORIENTED_EDGE('',*,*,#3071,.T.);
#3912=ORIENTED_EDGE('',*,*,#3074,.F.);
#3913=ORIENTED_EDGE('',*,*,#3073,.T.);
#3914=ORIENTED_EDGE('',*,*,#3075,.F.);
#3915=ORIENTED_EDGE('',*,*,#3076,.F.);
#3916=ORIENTED_EDGE('',*,*,#3077,.T.);
#3917=ORIENTED_EDGE('',*,*,#3075,.T.);
#3918=ORIENTED_EDGE('',*,*,#3077,.F.);
#3919=ORIENTED_EDGE('',*,*,#3067,.T.);
#3920=ORIENTED_EDGE('',*,*,#3078,.T.);
#3921=ORIENTED_EDGE('',*,*,#3076,.T.);
#3922=ORIENTED_EDGE('',*,*,#3078,.F.);
#3923=ORIENTED_EDGE('',*,*,#3079,.F.);
#3924=ORIENTED_EDGE('',*,*,#3080,.F.);
#3925=ORIENTED_EDGE('',*,*,#3081,.T.);
#3926=ORIENTED_EDGE('',*,*,#3082,.F.);
#3927=ORIENTED_EDGE('',*,*,#3083,.F.);
#3928=ORIENTED_EDGE('',*,*,#3081,.F.);
#3929=ORIENTED_EDGE('',*,*,#3082,.T.);
#3930=ORIENTED_EDGE('',*,*,#3083,.T.);
#3931=ORIENTED_EDGE('',*,*,#3084,.T.);
#3932=ORIENTED_EDGE('',*,*,#3085,.T.);
#3933=ORIENTED_EDGE('',*,*,#3084,.F.);
#3934=ORIENTED_EDGE('',*,*,#3086,.T.);
#3935=ORIENTED_EDGE('',*,*,#3087,.T.);
#3936=ORIENTED_EDGE('',*,*,#3088,.F.);
#3937=ORIENTED_EDGE('',*,*,#3087,.F.);
#3938=ORIENTED_EDGE('',*,*,#3088,.T.);
#3939=ORIENTED_EDGE('',*,*,#3089,.T.);
#3940=ORIENTED_EDGE('',*,*,#3090,.F.);
#3941=ORIENTED_EDGE('',*,*,#3089,.F.);
#3942=ORIENTED_EDGE('',*,*,#3085,.F.);
#3943=ORIENTED_EDGE('',*,*,#3090,.T.);
#3944=ORIENTED_EDGE('',*,*,#3091,.F.);
#3945=ORIENTED_EDGE('',*,*,#3092,.T.);
#3946=ORIENTED_EDGE('',*,*,#3079,.T.);
#3947=ORIENTED_EDGE('',*,*,#3080,.T.);
#3948=ORIENTED_EDGE('',*,*,#3092,.F.);
#3949=ORIENTED_EDGE('',*,*,#3091,.T.);
#3950=ORIENTED_EDGE('',*,*,#3093,.F.);
#3951=ORIENTED_EDGE('',*,*,#3093,.T.);
#3952=ORIENTED_EDGE('',*,*,#3094,.T.);
#3953=ORIENTED_EDGE('',*,*,#3086,.F.);
#3954=ORIENTED_EDGE('',*,*,#3094,.F.);
#3955=ORIENTED_EDGE('',*,*,#3095,.F.);
#3956=ORIENTED_EDGE('',*,*,#3096,.F.);
#3957=ORIENTED_EDGE('',*,*,#3097,.T.);
#3958=ORIENTED_EDGE('',*,*,#3098,.F.);
#3959=ORIENTED_EDGE('',*,*,#3099,.F.);
#3960=ORIENTED_EDGE('',*,*,#3097,.F.);
#3961=ORIENTED_EDGE('',*,*,#3100,.T.);
#3962=ORIENTED_EDGE('',*,*,#3101,.T.);
#3963=ORIENTED_EDGE('',*,*,#3098,.T.);
#3964=ORIENTED_EDGE('',*,*,#3099,.T.);
#3965=ORIENTED_EDGE('',*,*,#3101,.F.);
#3966=ORIENTED_EDGE('',*,*,#3102,.F.);
#3967=ORIENTED_EDGE('',*,*,#3103,.T.);
#3968=ORIENTED_EDGE('',*,*,#3104,.F.);
#3969=ORIENTED_EDGE('',*,*,#3105,.T.);
#3970=ORIENTED_EDGE('',*,*,#3102,.T.);
#3971=ORIENTED_EDGE('',*,*,#3105,.F.);
#3972=ORIENTED_EDGE('',*,*,#3106,.F.);
#3973=ORIENTED_EDGE('',*,*,#3107,.T.);
#3974=ORIENTED_EDGE('',*,*,#3104,.T.);
#3975=ORIENTED_EDGE('',*,*,#3107,.F.);
#3976=ORIENTED_EDGE('',*,*,#3108,.F.);
#3977=ORIENTED_EDGE('',*,*,#3109,.T.);
#3978=ORIENTED_EDGE('',*,*,#3106,.T.);
#3979=ORIENTED_EDGE('',*,*,#3109,.F.);
#3980=ORIENTED_EDGE('',*,*,#3108,.T.);
#3981=ORIENTED_EDGE('',*,*,#3100,.F.);
#3982=ORIENTED_EDGE('',*,*,#3095,.T.);
#3983=ORIENTED_EDGE('',*,*,#3096,.T.);
#3984=ORIENTED_EDGE('',*,*,#3110,.T.);
#3985=ORIENTED_EDGE('',*,*,#3103,.F.);
#3986=ORIENTED_EDGE('',*,*,#3110,.F.);
#3987=ORIENTED_EDGE('',*,*,#3111,.T.);
#3988=ORIENTED_EDGE('',*,*,#3111,.F.);
#3989=ORIENTED_EDGE('',*,*,#3112,.T.);
#3990=ORIENTED_EDGE('',*,*,#3112,.F.);
#3991=ORIENTED_EDGE('',*,*,#3113,.T.);
#3992=ORIENTED_EDGE('',*,*,#3113,.F.);
#3993=ORIENTED_EDGE('',*,*,#3114,.T.);
#3994=ORIENTED_EDGE('',*,*,#3114,.F.);
#3995=ORIENTED_EDGE('',*,*,#3115,.T.);
#3996=ORIENTED_EDGE('',*,*,#3115,.F.);
#3997=ORIENTED_EDGE('',*,*,#3116,.T.);
#3998=ORIENTED_EDGE('',*,*,#3116,.F.);
#3999=ORIENTED_EDGE('',*,*,#3117,.T.);
#4000=ORIENTED_EDGE('',*,*,#3117,.F.);
#4001=ORIENTED_EDGE('',*,*,#3118,.F.);
#4002=ORIENTED_EDGE('',*,*,#3119,.F.);
#4003=ORIENTED_EDGE('',*,*,#3120,.F.);
#4004=ORIENTED_EDGE('',*,*,#3121,.F.);
#4005=ORIENTED_EDGE('',*,*,#3120,.T.);
#4006=ORIENTED_EDGE('',*,*,#3122,.F.);
#4007=ORIENTED_EDGE('',*,*,#3123,.T.);
#4008=ORIENTED_EDGE('',*,*,#3124,.F.);
#4009=ORIENTED_EDGE('',*,*,#3125,.T.);
#4010=ORIENTED_EDGE('',*,*,#3126,.F.);
#4011=ORIENTED_EDGE('',*,*,#3127,.T.);
#4012=ORIENTED_EDGE('',*,*,#3128,.F.);
#4013=ORIENTED_EDGE('',*,*,#3127,.F.);
#4014=ORIENTED_EDGE('',*,*,#3129,.F.);
#4015=ORIENTED_EDGE('',*,*,#3130,.T.);
#4016=ORIENTED_EDGE('',*,*,#3131,.F.);
#4017=ORIENTED_EDGE('',*,*,#3132,.T.);
#4018=ORIENTED_EDGE('',*,*,#3133,.F.);
#4019=ORIENTED_EDGE('',*,*,#3134,.T.);
#4020=ORIENTED_EDGE('',*,*,#3135,.F.);
#4021=ORIENTED_EDGE('',*,*,#3136,.T.);
#4022=ORIENTED_EDGE('',*,*,#3137,.F.);
#4023=ORIENTED_EDGE('',*,*,#3119,.T.);
#4024=ORIENTED_EDGE('',*,*,#3138,.T.);
#4025=ORIENTED_EDGE('',*,*,#3139,.T.);
#4026=ORIENTED_EDGE('',*,*,#3122,.T.);
#4027=ORIENTED_EDGE('',*,*,#3140,.F.);
#4028=ORIENTED_EDGE('',*,*,#3141,.F.);
#4029=ORIENTED_EDGE('',*,*,#3123,.F.);
#4030=ORIENTED_EDGE('',*,*,#3139,.F.);
#4031=ORIENTED_EDGE('',*,*,#3141,.T.);
#4032=ORIENTED_EDGE('',*,*,#3142,.T.);
#4033=ORIENTED_EDGE('',*,*,#3143,.T.);
#4034=ORIENTED_EDGE('',*,*,#3124,.T.);
#4035=ORIENTED_EDGE('',*,*,#3144,.F.);
#4036=ORIENTED_EDGE('',*,*,#3145,.F.);
#4037=ORIENTED_EDGE('',*,*,#3125,.F.);
#4038=ORIENTED_EDGE('',*,*,#3143,.F.);
#4039=ORIENTED_EDGE('',*,*,#3145,.T.);
#4040=ORIENTED_EDGE('',*,*,#3146,.T.);
#4041=ORIENTED_EDGE('',*,*,#3147,.T.);
#4042=ORIENTED_EDGE('',*,*,#3148,.T.);
#4043=ORIENTED_EDGE('',*,*,#3129,.T.);
#4044=ORIENTED_EDGE('',*,*,#3126,.T.);
#4045=ORIENTED_EDGE('',*,*,#3149,.F.);
#4046=ORIENTED_EDGE('',*,*,#3150,.F.);
#4047=ORIENTED_EDGE('',*,*,#3130,.F.);
#4048=ORIENTED_EDGE('',*,*,#3148,.F.);
#4049=ORIENTED_EDGE('',*,*,#3150,.T.);
#4050=ORIENTED_EDGE('',*,*,#3151,.T.);
#4051=ORIENTED_EDGE('',*,*,#3152,.T.);
#4052=ORIENTED_EDGE('',*,*,#3131,.T.);
#4053=ORIENTED_EDGE('',*,*,#3153,.F.);
#4054=ORIENTED_EDGE('',*,*,#3154,.F.);
#4055=ORIENTED_EDGE('',*,*,#3132,.F.);
#4056=ORIENTED_EDGE('',*,*,#3152,.F.);
#4057=ORIENTED_EDGE('',*,*,#3154,.T.);
#4058=ORIENTED_EDGE('',*,*,#3155,.T.);
#4059=ORIENTED_EDGE('',*,*,#3156,.T.);
#4060=ORIENTED_EDGE('',*,*,#3133,.T.);
#4061=ORIENTED_EDGE('',*,*,#3134,.F.);
#4062=ORIENTED_EDGE('',*,*,#3156,.F.);
#4063=ORIENTED_EDGE('',*,*,#3157,.F.);
#4064=ORIENTED_EDGE('',*,*,#3158,.F.);
#4065=ORIENTED_EDGE('',*,*,#3159,.F.);
#4066=ORIENTED_EDGE('',*,*,#3160,.T.);
#4067=ORIENTED_EDGE('',*,*,#3146,.F.);
#4068=ORIENTED_EDGE('',*,*,#3144,.T.);
#4069=ORIENTED_EDGE('',*,*,#3142,.F.);
#4070=ORIENTED_EDGE('',*,*,#3140,.T.);
#4071=ORIENTED_EDGE('',*,*,#3138,.F.);
#4072=ORIENTED_EDGE('',*,*,#3118,.T.);
#4073=ORIENTED_EDGE('',*,*,#3161,.F.);
#4074=ORIENTED_EDGE('',*,*,#3162,.T.);
#4075=ORIENTED_EDGE('',*,*,#3163,.F.);
#4076=ORIENTED_EDGE('',*,*,#3157,.T.);
#4077=ORIENTED_EDGE('',*,*,#3155,.F.);
#4078=ORIENTED_EDGE('',*,*,#3153,.T.);
#4079=ORIENTED_EDGE('',*,*,#3151,.F.);
#4080=ORIENTED_EDGE('',*,*,#3149,.T.);
#4081=ORIENTED_EDGE('',*,*,#3147,.F.);
#4082=ORIENTED_EDGE('',*,*,#3160,.F.);
#4083=ORIENTED_EDGE('',*,*,#3121,.T.);
#4084=ORIENTED_EDGE('',*,*,#3137,.T.);
#4085=ORIENTED_EDGE('',*,*,#3164,.T.);
#4086=ORIENTED_EDGE('',*,*,#3161,.T.);
#4087=ORIENTED_EDGE('',*,*,#3136,.F.);
#4088=ORIENTED_EDGE('',*,*,#3165,.F.);
#4089=ORIENTED_EDGE('',*,*,#3162,.F.);
#4090=ORIENTED_EDGE('',*,*,#3164,.F.);
#4091=ORIENTED_EDGE('',*,*,#3128,.T.);
#4092=ORIENTED_EDGE('',*,*,#3159,.T.);
#4093=ORIENTED_EDGE('',*,*,#3158,.T.);
#4094=ORIENTED_EDGE('',*,*,#3163,.T.);
#4095=ORIENTED_EDGE('',*,*,#3165,.T.);
#4096=ORIENTED_EDGE('',*,*,#3135,.T.);
#4097=ORIENTED_EDGE('',*,*,#3166,.F.);
#4098=ORIENTED_EDGE('',*,*,#3167,.T.);
#4099=ORIENTED_EDGE('',*,*,#3168,.F.);
#4100=ORIENTED_EDGE('',*,*,#3169,.T.);
#4101=ORIENTED_EDGE('',*,*,#3166,.T.);
#4102=ORIENTED_EDGE('',*,*,#3169,.F.);
#4103=ORIENTED_EDGE('',*,*,#3168,.T.);
#4104=ORIENTED_EDGE('',*,*,#3170,.F.);
#4105=ORIENTED_EDGE('',*,*,#3170,.T.);
#4106=ORIENTED_EDGE('',*,*,#3171,.T.);
#4107=ORIENTED_EDGE('',*,*,#3167,.F.);
#4108=ORIENTED_EDGE('',*,*,#3171,.F.);
#4109=ORIENTED_EDGE('',*,*,#3172,.F.);
#4110=ORIENTED_EDGE('',*,*,#3173,.T.);
#4111=ORIENTED_EDGE('',*,*,#3174,.F.);
#4112=ORIENTED_EDGE('',*,*,#3175,.T.);
#4113=ORIENTED_EDGE('',*,*,#3172,.T.);
#4114=ORIENTED_EDGE('',*,*,#3175,.F.);
#4115=ORIENTED_EDGE('',*,*,#3174,.T.);
#4116=ORIENTED_EDGE('',*,*,#3176,.F.);
#4117=ORIENTED_EDGE('',*,*,#3176,.T.);
#4118=ORIENTED_EDGE('',*,*,#3177,.T.);
#4119=ORIENTED_EDGE('',*,*,#3173,.F.);
#4120=ORIENTED_EDGE('',*,*,#3177,.F.);
#4121=ORIENTED_EDGE('',*,*,#3178,.F.);
#4122=ORIENTED_EDGE('',*,*,#3179,.T.);
#4123=ORIENTED_EDGE('',*,*,#3180,.F.);
#4124=ORIENTED_EDGE('',*,*,#3181,.T.);
#4125=ORIENTED_EDGE('',*,*,#3182,.F.);
#4126=ORIENTED_EDGE('',*,*,#3181,.F.);
#4127=ORIENTED_EDGE('',*,*,#3183,.F.);
#4128=ORIENTED_EDGE('',*,*,#3184,.F.);
#4129=ORIENTED_EDGE('',*,*,#3185,.F.);
#4130=ORIENTED_EDGE('',*,*,#3184,.T.);
#4131=ORIENTED_EDGE('',*,*,#3186,.T.);
#4132=ORIENTED_EDGE('',*,*,#3187,.T.);
#4133=ORIENTED_EDGE('',*,*,#3183,.T.);
#4134=ORIENTED_EDGE('',*,*,#3180,.T.);
#4135=ORIENTED_EDGE('',*,*,#3188,.T.);
#4136=ORIENTED_EDGE('',*,*,#3186,.F.);
#4137=ORIENTED_EDGE('',*,*,#3189,.F.);
#4138=ORIENTED_EDGE('',*,*,#3187,.F.);
#4139=ORIENTED_EDGE('',*,*,#3188,.F.);
#4140=ORIENTED_EDGE('',*,*,#3179,.F.);
#4141=ORIENTED_EDGE('',*,*,#3190,.T.);
#4142=ORIENTED_EDGE('',*,*,#3191,.F.);
#4143=ORIENTED_EDGE('',*,*,#3192,.F.);
#4144=ORIENTED_EDGE('',*,*,#3193,.F.);
#4145=ORIENTED_EDGE('',*,*,#3190,.F.);
#4146=ORIENTED_EDGE('',*,*,#3194,.T.);
#4147=ORIENTED_EDGE('',*,*,#3192,.T.);
#4148=ORIENTED_EDGE('',*,*,#3194,.F.);
#4149=ORIENTED_EDGE('',*,*,#3193,.T.);
#4150=ORIENTED_EDGE('',*,*,#3195,.T.);
#4151=ORIENTED_EDGE('',*,*,#3196,.T.);
#4152=ORIENTED_EDGE('',*,*,#3195,.F.);
#4153=ORIENTED_EDGE('',*,*,#3185,.T.);
#4154=ORIENTED_EDGE('',*,*,#3189,.T.);
#4155=ORIENTED_EDGE('',*,*,#3178,.T.);
#4156=ORIENTED_EDGE('',*,*,#3182,.T.);
#4157=ORIENTED_EDGE('',*,*,#3197,.F.);
#4158=ORIENTED_EDGE('',*,*,#3198,.T.);
#4159=ORIENTED_EDGE('',*,*,#3191,.T.);
#4160=ORIENTED_EDGE('',*,*,#3198,.F.);
#4161=ORIENTED_EDGE('',*,*,#3197,.T.);
#4162=ORIENTED_EDGE('',*,*,#3196,.F.);
#4163=ORIENTED_EDGE('',*,*,#3199,.F.);
#4164=ORIENTED_EDGE('',*,*,#3200,.T.);
#4165=ORIENTED_EDGE('',*,*,#3201,.F.);
#4166=ORIENTED_EDGE('',*,*,#3200,.F.);
#4167=ORIENTED_EDGE('',*,*,#3202,.F.);
#4168=ORIENTED_EDGE('',*,*,#3203,.T.);
#4169=ORIENTED_EDGE('',*,*,#3204,.F.);
#4170=ORIENTED_EDGE('',*,*,#3203,.F.);
#4171=ORIENTED_EDGE('',*,*,#3205,.F.);
#4172=ORIENTED_EDGE('',*,*,#3206,.T.);
#4173=ORIENTED_EDGE('',*,*,#3207,.F.);
#4174=ORIENTED_EDGE('',*,*,#3208,.F.);
#4175=ORIENTED_EDGE('',*,*,#3209,.T.);
#4176=ORIENTED_EDGE('',*,*,#3210,.F.);
#4177=ORIENTED_EDGE('',*,*,#3211,.F.);
#4178=ORIENTED_EDGE('',*,*,#3209,.F.);
#4179=ORIENTED_EDGE('',*,*,#3212,.F.);
#4180=ORIENTED_EDGE('',*,*,#3213,.F.);
#4181=ORIENTED_EDGE('',*,*,#3206,.F.);
#4182=ORIENTED_EDGE('',*,*,#3214,.F.);
#4183=ORIENTED_EDGE('',*,*,#3212,.T.);
#4184=ORIENTED_EDGE('',*,*,#3208,.T.);
#4185=ORIENTED_EDGE('',*,*,#3215,.F.);
#4186=ORIENTED_EDGE('',*,*,#3216,.T.);
#4187=ORIENTED_EDGE('',*,*,#3217,.F.);
#4188=ORIENTED_EDGE('',*,*,#3218,.F.);
#4189=ORIENTED_EDGE('',*,*,#3219,.F.);
#4190=ORIENTED_EDGE('',*,*,#3220,.T.);
#4191=ORIENTED_EDGE('',*,*,#3221,.F.);
#4192=ORIENTED_EDGE('',*,*,#3216,.F.);
#4193=ORIENTED_EDGE('',*,*,#3222,.F.);
#4194=ORIENTED_EDGE('',*,*,#3223,.F.);
#4195=ORIENTED_EDGE('',*,*,#3224,.F.);
#4196=ORIENTED_EDGE('',*,*,#3220,.F.);
#4197=ORIENTED_EDGE('',*,*,#3225,.T.);
#4198=ORIENTED_EDGE('',*,*,#3217,.T.);
#4199=ORIENTED_EDGE('',*,*,#3221,.T.);
#4200=ORIENTED_EDGE('',*,*,#3224,.T.);
#4201=ORIENTED_EDGE('',*,*,#3226,.T.);
#4202=ORIENTED_EDGE('',*,*,#3218,.T.);
#4203=ORIENTED_EDGE('',*,*,#3226,.F.);
#4204=ORIENTED_EDGE('',*,*,#3223,.T.);
#4205=ORIENTED_EDGE('',*,*,#3227,.T.);
#4206=ORIENTED_EDGE('',*,*,#3213,.T.);
#4207=ORIENTED_EDGE('',*,*,#3214,.T.);
#4208=ORIENTED_EDGE('',*,*,#3207,.T.);
#4209=ORIENTED_EDGE('',*,*,#3205,.T.);
#4210=ORIENTED_EDGE('',*,*,#3228,.F.);
#4211=ORIENTED_EDGE('',*,*,#3229,.F.);
#4212=ORIENTED_EDGE('',*,*,#3230,.F.);
#4213=ORIENTED_EDGE('',*,*,#3231,.F.);
#4214=ORIENTED_EDGE('',*,*,#3232,.F.);
#4215=ORIENTED_EDGE('',*,*,#3233,.F.);
#4216=ORIENTED_EDGE('',*,*,#3234,.F.);
#4217=ORIENTED_EDGE('',*,*,#3235,.F.);
#4218=ORIENTED_EDGE('',*,*,#3236,.F.);
#4219=ORIENTED_EDGE('',*,*,#3199,.T.);
#4220=ORIENTED_EDGE('',*,*,#3202,.T.);
#4221=ORIENTED_EDGE('',*,*,#3237,.F.);
#4222=ORIENTED_EDGE('',*,*,#3238,.T.);
#4223=ORIENTED_EDGE('',*,*,#3239,.F.);
#4224=ORIENTED_EDGE('',*,*,#3240,.T.);
#4225=ORIENTED_EDGE('',*,*,#3241,.F.);
#4226=ORIENTED_EDGE('',*,*,#3242,.T.);
#4227=ORIENTED_EDGE('',*,*,#3243,.F.);
#4228=ORIENTED_EDGE('',*,*,#3244,.T.);
#4229=ORIENTED_EDGE('',*,*,#3245,.F.);
#4230=ORIENTED_EDGE('',*,*,#3231,.T.);
#4231=ORIENTED_EDGE('',*,*,#3246,.F.);
#4232=ORIENTED_EDGE('',*,*,#3233,.T.);
#4233=ORIENTED_EDGE('',*,*,#3232,.T.);
#4234=ORIENTED_EDGE('',*,*,#3247,.F.);
#4235=ORIENTED_EDGE('',*,*,#3248,.T.);
#4236=ORIENTED_EDGE('',*,*,#3237,.T.);
#4237=ORIENTED_EDGE('',*,*,#3248,.F.);
#4238=ORIENTED_EDGE('',*,*,#3249,.F.);
#4239=ORIENTED_EDGE('',*,*,#3250,.F.);
#4240=ORIENTED_EDGE('',*,*,#3238,.F.);
#4241=ORIENTED_EDGE('',*,*,#3251,.F.);
#4242=ORIENTED_EDGE('',*,*,#3240,.F.);
#4243=ORIENTED_EDGE('',*,*,#3252,.F.);
#4244=ORIENTED_EDGE('',*,*,#3253,.F.);
#4245=ORIENTED_EDGE('',*,*,#3251,.T.);
#4246=ORIENTED_EDGE('',*,*,#3254,.F.);
#4247=ORIENTED_EDGE('',*,*,#3255,.T.);
#4248=ORIENTED_EDGE('',*,*,#3241,.T.);
#4249=ORIENTED_EDGE('',*,*,#3256,.F.);
#4250=ORIENTED_EDGE('',*,*,#3242,.F.);
#4251=ORIENTED_EDGE('',*,*,#3255,.F.);
#4252=ORIENTED_EDGE('',*,*,#3257,.F.);
#4253=ORIENTED_EDGE('',*,*,#3258,.F.);
#4254=ORIENTED_EDGE('',*,*,#3259,.F.);
#4255=ORIENTED_EDGE('',*,*,#3260,.F.);
#4256=ORIENTED_EDGE('',*,*,#3244,.F.);
#4257=ORIENTED_EDGE('',*,*,#3261,.T.);
#4258=ORIENTED_EDGE('',*,*,#3201,.T.);
#4259=ORIENTED_EDGE('',*,*,#3204,.T.);
#4260=ORIENTED_EDGE('',*,*,#3262,.T.);
#4261=ORIENTED_EDGE('',*,*,#3259,.T.);
#4262=ORIENTED_EDGE('',*,*,#3263,.F.);
#4263=ORIENTED_EDGE('',*,*,#3257,.T.);
#4264=ORIENTED_EDGE('',*,*,#3254,.T.);
#4265=ORIENTED_EDGE('',*,*,#3253,.T.);
#4266=ORIENTED_EDGE('',*,*,#3264,.F.);
#4267=ORIENTED_EDGE('',*,*,#3249,.T.);
#4268=ORIENTED_EDGE('',*,*,#3247,.T.);
#4269=ORIENTED_EDGE('',*,*,#3235,.T.);
#4270=ORIENTED_EDGE('',*,*,#3265,.F.);
#4271=ORIENTED_EDGE('',*,*,#3229,.T.);
#4272=ORIENTED_EDGE('',*,*,#3228,.T.);
#4273=ORIENTED_EDGE('',*,*,#3245,.T.);
#4274=ORIENTED_EDGE('',*,*,#3260,.T.);
#4275=ORIENTED_EDGE('',*,*,#3262,.F.);
#4276=ORIENTED_EDGE('',*,*,#3261,.F.);
#4277=ORIENTED_EDGE('',*,*,#3266,.T.);
#4278=ORIENTED_EDGE('',*,*,#3236,.T.);
#4279=ORIENTED_EDGE('',*,*,#3266,.F.);
#4280=ORIENTED_EDGE('',*,*,#3225,.F.);
#4281=ORIENTED_EDGE('',*,*,#3267,.T.);
#4282=ORIENTED_EDGE('',*,*,#3268,.T.);
#4283=ORIENTED_EDGE('',*,*,#3267,.F.);
#4284=ORIENTED_EDGE('',*,*,#3210,.T.);
#4285=ORIENTED_EDGE('',*,*,#3211,.T.);
#4286=ORIENTED_EDGE('',*,*,#3230,.T.);
#4287=ORIENTED_EDGE('',*,*,#3265,.T.);
#4288=ORIENTED_EDGE('',*,*,#3234,.T.);
#4289=ORIENTED_EDGE('',*,*,#3246,.T.);
#4290=ORIENTED_EDGE('',*,*,#3250,.T.);
#4291=ORIENTED_EDGE('',*,*,#3264,.T.);
#4292=ORIENTED_EDGE('',*,*,#3252,.T.);
#4293=ORIENTED_EDGE('',*,*,#3239,.T.);
#4294=ORIENTED_EDGE('',*,*,#3256,.T.);
#4295=ORIENTED_EDGE('',*,*,#3263,.T.);
#4296=ORIENTED_EDGE('',*,*,#3258,.T.);
#4297=ORIENTED_EDGE('',*,*,#3243,.T.);
#4298=ORIENTED_EDGE('',*,*,#3268,.F.);
#4299=ORIENTED_EDGE('',*,*,#3215,.T.);
#4300=ORIENTED_EDGE('',*,*,#3227,.F.);
#4301=ORIENTED_EDGE('',*,*,#3222,.T.);
#4302=ORIENTED_EDGE('',*,*,#3219,.T.);
#4303=ORIENTED_EDGE('',*,*,#3269,.F.);
#4304=ORIENTED_EDGE('',*,*,#3270,.T.);
#4305=ORIENTED_EDGE('',*,*,#3271,.T.);
#4306=ORIENTED_EDGE('',*,*,#3270,.F.);
#4307=ORIENTED_EDGE('',*,*,#3272,.F.);
#4308=ORIENTED_EDGE('',*,*,#3273,.T.);
#4309=ORIENTED_EDGE('',*,*,#3274,.T.);
#4310=ORIENTED_EDGE('',*,*,#3273,.F.);
#4311=ORIENTED_EDGE('',*,*,#3272,.T.);
#4312=ORIENTED_EDGE('',*,*,#3269,.T.);
#4313=ORIENTED_EDGE('',*,*,#3274,.F.);
#4314=ORIENTED_EDGE('',*,*,#3271,.F.);
#4315=ORIENTED_EDGE('',*,*,#3275,.F.);
#4316=ORIENTED_EDGE('',*,*,#3276,.T.);
#4317=ORIENTED_EDGE('',*,*,#3277,.F.);
#4318=ORIENTED_EDGE('',*,*,#3278,.F.);
#4319=ORIENTED_EDGE('',*,*,#3279,.T.);
#4320=ORIENTED_EDGE('',*,*,#3280,.F.);
#4321=ORIENTED_EDGE('',*,*,#3281,.F.);
#4322=ORIENTED_EDGE('',*,*,#3279,.F.);
#4323=ORIENTED_EDGE('',*,*,#3282,.F.);
#4324=ORIENTED_EDGE('',*,*,#3283,.F.);
#4325=ORIENTED_EDGE('',*,*,#3276,.F.);
#4326=ORIENTED_EDGE('',*,*,#3284,.F.);
#4327=ORIENTED_EDGE('',*,*,#3282,.T.);
#4328=ORIENTED_EDGE('',*,*,#3278,.T.);
#4329=ORIENTED_EDGE('',*,*,#3285,.F.);
#4330=ORIENTED_EDGE('',*,*,#3286,.T.);
#4331=ORIENTED_EDGE('',*,*,#3287,.T.);
#4332=ORIENTED_EDGE('',*,*,#3286,.F.);
#4333=ORIENTED_EDGE('',*,*,#3283,.T.);
#4334=ORIENTED_EDGE('',*,*,#3284,.T.);
#4335=ORIENTED_EDGE('',*,*,#3277,.T.);
#4336=ORIENTED_EDGE('',*,*,#3275,.T.);
#4337=ORIENTED_EDGE('',*,*,#3288,.F.);
#4338=ORIENTED_EDGE('',*,*,#3289,.T.);
#4339=ORIENTED_EDGE('',*,*,#3290,.T.);
#4340=ORIENTED_EDGE('',*,*,#3289,.F.);
#4341=ORIENTED_EDGE('',*,*,#3280,.T.);
#4342=ORIENTED_EDGE('',*,*,#3281,.T.);
#4343=ORIENTED_EDGE('',*,*,#3288,.T.);
#4344=ORIENTED_EDGE('',*,*,#3285,.T.);
#4345=ORIENTED_EDGE('',*,*,#3290,.F.);
#4346=ORIENTED_EDGE('',*,*,#3287,.F.);
#4347=ORIENTED_EDGE('',*,*,#3291,.F.);
#4348=ORIENTED_EDGE('',*,*,#3292,.T.);
#4349=ORIENTED_EDGE('',*,*,#3293,.T.);
#4350=ORIENTED_EDGE('',*,*,#3292,.F.);
#4351=ORIENTED_EDGE('',*,*,#3293,.F.);
#4352=ORIENTED_EDGE('',*,*,#3294,.F.);
#4353=ORIENTED_EDGE('',*,*,#3295,.T.);
#4354=ORIENTED_EDGE('',*,*,#3296,.F.);
#4355=ORIENTED_EDGE('',*,*,#3295,.F.);
#4356=ORIENTED_EDGE('',*,*,#3297,.F.);
#4357=ORIENTED_EDGE('',*,*,#3298,.T.);
#4358=ORIENTED_EDGE('',*,*,#3299,.F.);
#4359=ORIENTED_EDGE('',*,*,#3298,.F.);
#4360=ORIENTED_EDGE('',*,*,#3300,.F.);
#4361=ORIENTED_EDGE('',*,*,#3294,.T.);
#4362=ORIENTED_EDGE('',*,*,#3297,.T.);
#4363=ORIENTED_EDGE('',*,*,#3301,.F.);
#4364=ORIENTED_EDGE('',*,*,#3302,.F.);
#4365=ORIENTED_EDGE('',*,*,#3303,.T.);
#4366=ORIENTED_EDGE('',*,*,#3300,.T.);
#4367=ORIENTED_EDGE('',*,*,#3303,.F.);
#4368=ORIENTED_EDGE('',*,*,#3304,.F.);
#4369=ORIENTED_EDGE('',*,*,#3305,.F.);
#4370=ORIENTED_EDGE('',*,*,#3301,.T.);
#4371=ORIENTED_EDGE('',*,*,#3306,.T.);
#4372=ORIENTED_EDGE('',*,*,#3304,.T.);
#4373=ORIENTED_EDGE('',*,*,#3306,.F.);
#4374=ORIENTED_EDGE('',*,*,#3305,.T.);
#4375=ORIENTED_EDGE('',*,*,#3307,.T.);
#4376=ORIENTED_EDGE('',*,*,#3308,.T.);
#4377=ORIENTED_EDGE('',*,*,#3307,.F.);
#4378=ORIENTED_EDGE('',*,*,#3302,.T.);
#4379=ORIENTED_EDGE('',*,*,#3296,.T.);
#4380=ORIENTED_EDGE('',*,*,#3299,.T.);
#4381=ORIENTED_EDGE('',*,*,#3308,.F.);
#4382=ORIENTED_EDGE('',*,*,#3291,.T.);
#4383=ORIENTED_EDGE('',*,*,#3309,.F.);
#4384=ORIENTED_EDGE('',*,*,#3310,.T.);
#4385=ORIENTED_EDGE('',*,*,#3311,.T.);
#4386=ORIENTED_EDGE('',*,*,#3310,.F.);
#4387=ORIENTED_EDGE('',*,*,#3312,.F.);
#4388=ORIENTED_EDGE('',*,*,#3313,.T.);
#4389=ORIENTED_EDGE('',*,*,#3314,.T.);
#4390=ORIENTED_EDGE('',*,*,#3313,.F.);
#4391=ORIENTED_EDGE('',*,*,#3312,.T.);
#4392=ORIENTED_EDGE('',*,*,#3309,.T.);
#4393=ORIENTED_EDGE('',*,*,#3314,.F.);
#4394=ORIENTED_EDGE('',*,*,#3311,.F.);
#4395=ORIENTED_EDGE('',*,*,#3315,.F.);
#4396=ORIENTED_EDGE('',*,*,#3316,.T.);
#4397=ORIENTED_EDGE('',*,*,#3317,.T.);
#4398=ORIENTED_EDGE('',*,*,#3316,.F.);
#4399=ORIENTED_EDGE('',*,*,#3318,.F.);
#4400=ORIENTED_EDGE('',*,*,#3319,.T.);
#4401=ORIENTED_EDGE('',*,*,#3320,.T.);
#4402=ORIENTED_EDGE('',*,*,#3319,.F.);
#4403=ORIENTED_EDGE('',*,*,#3318,.T.);
#4404=ORIENTED_EDGE('',*,*,#3315,.T.);
#4405=ORIENTED_EDGE('',*,*,#3320,.F.);
#4406=ORIENTED_EDGE('',*,*,#3317,.F.);
#4407=ORIENTED_EDGE('',*,*,#3321,.T.);
#4408=ORIENTED_EDGE('',*,*,#3322,.T.);
#4409=ORIENTED_EDGE('',*,*,#3323,.T.);
#4410=ORIENTED_EDGE('',*,*,#3324,.T.);
#4411=ORIENTED_EDGE('',*,*,#3325,.T.);
#4412=ORIENTED_EDGE('',*,*,#3326,.T.);
#4413=ORIENTED_EDGE('',*,*,#3321,.F.);
#4414=ORIENTED_EDGE('',*,*,#3327,.T.);
#4415=ORIENTED_EDGE('',*,*,#3328,.T.);
#4416=ORIENTED_EDGE('',*,*,#3329,.T.);
#4417=ORIENTED_EDGE('',*,*,#3325,.F.);
#4418=ORIENTED_EDGE('',*,*,#3330,.T.);
#4419=ORIENTED_EDGE('',*,*,#3323,.F.);
#4420=ORIENTED_EDGE('',*,*,#3331,.T.);
#4421=ORIENTED_EDGE('',*,*,#3328,.F.);
#4422=ORIENTED_EDGE('',*,*,#3332,.T.);
#4423=ORIENTED_EDGE('',*,*,#3327,.F.);
#4424=ORIENTED_EDGE('',*,*,#3333,.F.);
#4425=ORIENTED_EDGE('',*,*,#3334,.F.);
#4426=ORIENTED_EDGE('',*,*,#3335,.T.);
#4427=ORIENTED_EDGE('',*,*,#3324,.F.);
#4428=ORIENTED_EDGE('',*,*,#3336,.F.);
#4429=ORIENTED_EDGE('',*,*,#3337,.F.);
#4430=ORIENTED_EDGE('',*,*,#3333,.T.);
#4431=ORIENTED_EDGE('',*,*,#3322,.F.);
#4432=ORIENTED_EDGE('',*,*,#3326,.F.);
#4433=ORIENTED_EDGE('',*,*,#3329,.F.);
#4434=ORIENTED_EDGE('',*,*,#3331,.F.);
#4435=ORIENTED_EDGE('',*,*,#3338,.T.);
#4436=ORIENTED_EDGE('',*,*,#3337,.T.);
#4437=ORIENTED_EDGE('',*,*,#3339,.T.);
#4438=ORIENTED_EDGE('',*,*,#3340,.T.);
#4439=ORIENTED_EDGE('',*,*,#3341,.T.);
#4440=ORIENTED_EDGE('',*,*,#3334,.T.);
#4441=ORIENTED_EDGE('',*,*,#3338,.F.);
#4442=ORIENTED_EDGE('',*,*,#3342,.T.);
#4443=ORIENTED_EDGE('',*,*,#3343,.T.);
#4444=ORIENTED_EDGE('',*,*,#3344,.T.);
#4445=ORIENTED_EDGE('',*,*,#3341,.F.);
#4446=ORIENTED_EDGE('',*,*,#3345,.T.);
#4447=ORIENTED_EDGE('',*,*,#3339,.F.);
#4448=ORIENTED_EDGE('',*,*,#3346,.T.);
#4449=ORIENTED_EDGE('',*,*,#3343,.F.);
#4450=ORIENTED_EDGE('',*,*,#3347,.T.);
#4451=ORIENTED_EDGE('',*,*,#3332,.F.);
#4452=ORIENTED_EDGE('',*,*,#3348,.F.);
#4453=ORIENTED_EDGE('',*,*,#3346,.F.);
#4454=ORIENTED_EDGE('',*,*,#3336,.T.);
#4455=ORIENTED_EDGE('',*,*,#3340,.F.);
#4456=ORIENTED_EDGE('',*,*,#3347,.F.);
#4457=ORIENTED_EDGE('',*,*,#3345,.F.);
#4458=ORIENTED_EDGE('',*,*,#3342,.F.);
#4459=ORIENTED_EDGE('',*,*,#3330,.F.);
#4460=ORIENTED_EDGE('',*,*,#3335,.F.);
#4461=ORIENTED_EDGE('',*,*,#3344,.F.);
#4462=ORIENTED_EDGE('',*,*,#3348,.T.);
#4463=ORIENTED_EDGE('',*,*,#3349,.F.);
#4464=ORIENTED_EDGE('',*,*,#3350,.T.);
#4465=ORIENTED_EDGE('',*,*,#3351,.T.);
#4466=ORIENTED_EDGE('',*,*,#3352,.F.);
#4467=ORIENTED_EDGE('',*,*,#3353,.F.);
#4468=ORIENTED_EDGE('',*,*,#3354,.T.);
#4469=ORIENTED_EDGE('',*,*,#3355,.T.);
#4470=ORIENTED_EDGE('',*,*,#3350,.F.);
#4471=ORIENTED_EDGE('',*,*,#3356,.F.);
#4472=ORIENTED_EDGE('',*,*,#3357,.T.);
#4473=ORIENTED_EDGE('',*,*,#3358,.T.);
#4474=ORIENTED_EDGE('',*,*,#3354,.F.);
#4475=ORIENTED_EDGE('',*,*,#3359,.F.);
#4476=ORIENTED_EDGE('',*,*,#3360,.T.);
#4477=ORIENTED_EDGE('',*,*,#3361,.T.);
#4478=ORIENTED_EDGE('',*,*,#3357,.F.);
#4479=ORIENTED_EDGE('',*,*,#3362,.F.);
#4480=ORIENTED_EDGE('',*,*,#3363,.T.);
#4481=ORIENTED_EDGE('',*,*,#3364,.T.);
#4482=ORIENTED_EDGE('',*,*,#3360,.F.);
#4483=ORIENTED_EDGE('',*,*,#3365,.F.);
#4484=ORIENTED_EDGE('',*,*,#3352,.T.);
#4485=ORIENTED_EDGE('',*,*,#3366,.T.);
#4486=ORIENTED_EDGE('',*,*,#3363,.F.);
#4487=ORIENTED_EDGE('',*,*,#3366,.F.);
#4488=ORIENTED_EDGE('',*,*,#3351,.F.);
#4489=ORIENTED_EDGE('',*,*,#3355,.F.);
#4490=ORIENTED_EDGE('',*,*,#3358,.F.);
#4491=ORIENTED_EDGE('',*,*,#3361,.F.);
#4492=ORIENTED_EDGE('',*,*,#3364,.F.);
#4493=ORIENTED_EDGE('',*,*,#3367,.F.);
#4494=ORIENTED_EDGE('',*,*,#3349,.T.);
#4495=ORIENTED_EDGE('',*,*,#3365,.T.);
#4496=ORIENTED_EDGE('',*,*,#3362,.T.);
#4497=ORIENTED_EDGE('',*,*,#3359,.T.);
#4498=ORIENTED_EDGE('',*,*,#3356,.T.);
#4499=ORIENTED_EDGE('',*,*,#3353,.T.);
#4500=ORIENTED_EDGE('',*,*,#3368,.F.);
#4501=ORIENTED_EDGE('',*,*,#3369,.T.);
#4502=ORIENTED_EDGE('',*,*,#3367,.T.);
#4503=ORIENTED_EDGE('',*,*,#3369,.F.);
#4504=ORIENTED_EDGE('',*,*,#3370,.F.);
#4505=ORIENTED_EDGE('',*,*,#3371,.T.);
#4506=ORIENTED_EDGE('',*,*,#3368,.T.);
#4507=ORIENTED_EDGE('',*,*,#3371,.F.);
#4508=ORIENTED_EDGE('',*,*,#3372,.F.);
#4509=ORIENTED_EDGE('',*,*,#3373,.T.);
#4510=ORIENTED_EDGE('',*,*,#3370,.T.);
#4511=ORIENTED_EDGE('',*,*,#3373,.F.);
#4512=ORIENTED_EDGE('',*,*,#3372,.T.);
#4513=ORIENTED_EDGE('',*,*,#3374,.T.);
#4514=ORIENTED_EDGE('',*,*,#3375,.T.);
#4515=ORIENTED_EDGE('',*,*,#3376,.T.);
#4516=ORIENTED_EDGE('',*,*,#3377,.F.);
#4517=ORIENTED_EDGE('',*,*,#3378,.T.);
#4518=ORIENTED_EDGE('',*,*,#3379,.T.);
#4519=ORIENTED_EDGE('',*,*,#3380,.T.);
#4520=ORIENTED_EDGE('',*,*,#3375,.F.);
#4521=ORIENTED_EDGE('',*,*,#3381,.T.);
#4522=ORIENTED_EDGE('',*,*,#3382,.T.);
#4523=ORIENTED_EDGE('',*,*,#3383,.T.);
#4524=ORIENTED_EDGE('',*,*,#3379,.F.);
#4525=ORIENTED_EDGE('',*,*,#3384,.T.);
#4526=ORIENTED_EDGE('',*,*,#3385,.T.);
#4527=ORIENTED_EDGE('',*,*,#3386,.T.);
#4528=ORIENTED_EDGE('',*,*,#3382,.F.);
#4529=ORIENTED_EDGE('',*,*,#3387,.T.);
#4530=ORIENTED_EDGE('',*,*,#3388,.T.);
#4531=ORIENTED_EDGE('',*,*,#3389,.T.);
#4532=ORIENTED_EDGE('',*,*,#3385,.F.);
#4533=ORIENTED_EDGE('',*,*,#3390,.T.);
#4534=ORIENTED_EDGE('',*,*,#3377,.T.);
#4535=ORIENTED_EDGE('',*,*,#3391,.T.);
#4536=ORIENTED_EDGE('',*,*,#3388,.F.);
#4537=ORIENTED_EDGE('',*,*,#3390,.F.);
#4538=ORIENTED_EDGE('',*,*,#3387,.F.);
#4539=ORIENTED_EDGE('',*,*,#3384,.F.);
#4540=ORIENTED_EDGE('',*,*,#3381,.F.);
#4541=ORIENTED_EDGE('',*,*,#3378,.F.);
#4542=ORIENTED_EDGE('',*,*,#3374,.F.);
#4543=ORIENTED_EDGE('',*,*,#3391,.F.);
#4544=ORIENTED_EDGE('',*,*,#3376,.F.);
#4545=ORIENTED_EDGE('',*,*,#3380,.F.);
#4546=ORIENTED_EDGE('',*,*,#3383,.F.);
#4547=ORIENTED_EDGE('',*,*,#3386,.F.);
#4548=ORIENTED_EDGE('',*,*,#3389,.F.);
#4549=ORIENTED_EDGE('',*,*,#3392,.F.);
#4550=ORIENTED_EDGE('',*,*,#3393,.F.);
#4551=ORIENTED_EDGE('',*,*,#3394,.F.);
#4552=ORIENTED_EDGE('',*,*,#3395,.T.);
#4553=ORIENTED_EDGE('',*,*,#3393,.T.);
#4554=ORIENTED_EDGE('',*,*,#3395,.F.);
#4555=ORIENTED_EDGE('',*,*,#3396,.F.);
#4556=ORIENTED_EDGE('',*,*,#3397,.T.);
#4557=ORIENTED_EDGE('',*,*,#3394,.T.);
#4558=ORIENTED_EDGE('',*,*,#3397,.F.);
#4559=ORIENTED_EDGE('',*,*,#3398,.F.);
#4560=ORIENTED_EDGE('',*,*,#3399,.T.);
#4561=ORIENTED_EDGE('',*,*,#3396,.T.);
#4562=ORIENTED_EDGE('',*,*,#3399,.F.);
#4563=ORIENTED_EDGE('',*,*,#3398,.T.);
#4564=ORIENTED_EDGE('',*,*,#3400,.F.);
#4565=ORIENTED_EDGE('',*,*,#3401,.F.);
#4566=ORIENTED_EDGE('',*,*,#3402,.T.);
#4567=ORIENTED_EDGE('',*,*,#3400,.T.);
#4568=ORIENTED_EDGE('',*,*,#3402,.F.);
#4569=ORIENTED_EDGE('',*,*,#3392,.T.);
#4570=ORIENTED_EDGE('',*,*,#3403,.T.);
#4571=ORIENTED_EDGE('',*,*,#3401,.T.);
#4572=ORIENTED_EDGE('',*,*,#3403,.F.);
#4573=ORIENTED_EDGE('',*,*,#3404,.F.);
#4574=ORIENTED_EDGE('',*,*,#3405,.F.);
#4575=ORIENTED_EDGE('',*,*,#3406,.T.);
#4576=ORIENTED_EDGE('',*,*,#3407,.F.);
#4577=ORIENTED_EDGE('',*,*,#3408,.F.);
#4578=ORIENTED_EDGE('',*,*,#3406,.F.);
#4579=ORIENTED_EDGE('',*,*,#3407,.T.);
#4580=ORIENTED_EDGE('',*,*,#3408,.T.);
#4581=ORIENTED_EDGE('',*,*,#3409,.T.);
#4582=ORIENTED_EDGE('',*,*,#3410,.T.);
#4583=ORIENTED_EDGE('',*,*,#3409,.F.);
#4584=ORIENTED_EDGE('',*,*,#3411,.T.);
#4585=ORIENTED_EDGE('',*,*,#3412,.T.);
#4586=ORIENTED_EDGE('',*,*,#3413,.F.);
#4587=ORIENTED_EDGE('',*,*,#3412,.F.);
#4588=ORIENTED_EDGE('',*,*,#3413,.T.);
#4589=ORIENTED_EDGE('',*,*,#3414,.T.);
#4590=ORIENTED_EDGE('',*,*,#3415,.F.);
#4591=ORIENTED_EDGE('',*,*,#3414,.F.);
#4592=ORIENTED_EDGE('',*,*,#3410,.F.);
#4593=ORIENTED_EDGE('',*,*,#3415,.T.);
#4594=ORIENTED_EDGE('',*,*,#3416,.F.);
#4595=ORIENTED_EDGE('',*,*,#3417,.T.);
#4596=ORIENTED_EDGE('',*,*,#3404,.T.);
#4597=ORIENTED_EDGE('',*,*,#3405,.T.);
#4598=ORIENTED_EDGE('',*,*,#3417,.F.);
#4599=ORIENTED_EDGE('',*,*,#3416,.T.);
#4600=ORIENTED_EDGE('',*,*,#3418,.F.);
#4601=ORIENTED_EDGE('',*,*,#3418,.T.);
#4602=ORIENTED_EDGE('',*,*,#3419,.T.);
#4603=ORIENTED_EDGE('',*,*,#3411,.F.);
#4604=ORIENTED_EDGE('',*,*,#3419,.F.);
#4605=ORIENTED_EDGE('',*,*,#3420,.F.);
#4606=ORIENTED_EDGE('',*,*,#3421,.F.);
#4607=ORIENTED_EDGE('',*,*,#3422,.T.);
#4608=ORIENTED_EDGE('',*,*,#3423,.F.);
#4609=ORIENTED_EDGE('',*,*,#3424,.F.);
#4610=ORIENTED_EDGE('',*,*,#3422,.F.);
#4611=ORIENTED_EDGE('',*,*,#3425,.T.);
#4612=ORIENTED_EDGE('',*,*,#3426,.T.);
#4613=ORIENTED_EDGE('',*,*,#3423,.T.);
#4614=ORIENTED_EDGE('',*,*,#3424,.T.);
#4615=ORIENTED_EDGE('',*,*,#3426,.F.);
#4616=ORIENTED_EDGE('',*,*,#3427,.F.);
#4617=ORIENTED_EDGE('',*,*,#3428,.T.);
#4618=ORIENTED_EDGE('',*,*,#3429,.F.);
#4619=ORIENTED_EDGE('',*,*,#3430,.T.);
#4620=ORIENTED_EDGE('',*,*,#3427,.T.);
#4621=ORIENTED_EDGE('',*,*,#3430,.F.);
#4622=ORIENTED_EDGE('',*,*,#3431,.F.);
#4623=ORIENTED_EDGE('',*,*,#3432,.T.);
#4624=ORIENTED_EDGE('',*,*,#3429,.T.);
#4625=ORIENTED_EDGE('',*,*,#3432,.F.);
#4626=ORIENTED_EDGE('',*,*,#3433,.F.);
#4627=ORIENTED_EDGE('',*,*,#3434,.T.);
#4628=ORIENTED_EDGE('',*,*,#3431,.T.);
#4629=ORIENTED_EDGE('',*,*,#3434,.F.);
#4630=ORIENTED_EDGE('',*,*,#3433,.T.);
#4631=ORIENTED_EDGE('',*,*,#3425,.F.);
#4632=ORIENTED_EDGE('',*,*,#3420,.T.);
#4633=ORIENTED_EDGE('',*,*,#3421,.T.);
#4634=ORIENTED_EDGE('',*,*,#3435,.T.);
#4635=ORIENTED_EDGE('',*,*,#3428,.F.);
#4636=ORIENTED_EDGE('',*,*,#3435,.F.);
#4637=ORIENTED_EDGE('',*,*,#3436,.T.);
#4638=ORIENTED_EDGE('',*,*,#3436,.F.);
#4639=ORIENTED_EDGE('',*,*,#3437,.T.);
#4640=ORIENTED_EDGE('',*,*,#3437,.F.);
#4641=ORIENTED_EDGE('',*,*,#3438,.T.);
#4642=ORIENTED_EDGE('',*,*,#3438,.F.);
#4643=ORIENTED_EDGE('',*,*,#3439,.T.);
#4644=ORIENTED_EDGE('',*,*,#3439,.F.);
#4645=ORIENTED_EDGE('',*,*,#3440,.T.);
#4646=ORIENTED_EDGE('',*,*,#3440,.F.);
#4647=ORIENTED_EDGE('',*,*,#3441,.T.);
#4648=ORIENTED_EDGE('',*,*,#3441,.F.);
#4649=ORIENTED_EDGE('',*,*,#3442,.T.);
#4650=ORIENTED_EDGE('',*,*,#3442,.F.);
#4651=ORIENTED_EDGE('',*,*,#3443,.T.);
#4652=ORIENTED_EDGE('',*,*,#3443,.F.);
#4653=ORIENTED_EDGE('',*,*,#3444,.F.);
#4654=ORIENTED_EDGE('',*,*,#3445,.F.);
#4655=ORIENTED_EDGE('',*,*,#3446,.F.);
#4656=ORIENTED_EDGE('',*,*,#3447,.F.);
#4657=ORIENTED_EDGE('',*,*,#3446,.T.);
#4658=ORIENTED_EDGE('',*,*,#3448,.F.);
#4659=ORIENTED_EDGE('',*,*,#3449,.T.);
#4660=ORIENTED_EDGE('',*,*,#3450,.F.);
#4661=ORIENTED_EDGE('',*,*,#3451,.T.);
#4662=ORIENTED_EDGE('',*,*,#3452,.F.);
#4663=ORIENTED_EDGE('',*,*,#3453,.T.);
#4664=ORIENTED_EDGE('',*,*,#3454,.T.);
#4665=ORIENTED_EDGE('',*,*,#3455,.F.);
#4666=ORIENTED_EDGE('',*,*,#3454,.F.);
#4667=ORIENTED_EDGE('',*,*,#3456,.T.);
#4668=ORIENTED_EDGE('',*,*,#3457,.F.);
#4669=ORIENTED_EDGE('',*,*,#3458,.T.);
#4670=ORIENTED_EDGE('',*,*,#3459,.F.);
#4671=ORIENTED_EDGE('',*,*,#3460,.T.);
#4672=ORIENTED_EDGE('',*,*,#3461,.F.);
#4673=ORIENTED_EDGE('',*,*,#3462,.T.);
#4674=ORIENTED_EDGE('',*,*,#3463,.F.);
#4675=ORIENTED_EDGE('',*,*,#3464,.T.);
#4676=ORIENTED_EDGE('',*,*,#3465,.F.);
#4677=ORIENTED_EDGE('',*,*,#3445,.T.);
#4678=ORIENTED_EDGE('',*,*,#3466,.T.);
#4679=ORIENTED_EDGE('',*,*,#3467,.T.);
#4680=ORIENTED_EDGE('',*,*,#3448,.T.);
#4681=ORIENTED_EDGE('',*,*,#3468,.F.);
#4682=ORIENTED_EDGE('',*,*,#3469,.F.);
#4683=ORIENTED_EDGE('',*,*,#3449,.F.);
#4684=ORIENTED_EDGE('',*,*,#3467,.F.);
#4685=ORIENTED_EDGE('',*,*,#3469,.T.);
#4686=ORIENTED_EDGE('',*,*,#3470,.T.);
#4687=ORIENTED_EDGE('',*,*,#3471,.T.);
#4688=ORIENTED_EDGE('',*,*,#3450,.T.);
#4689=ORIENTED_EDGE('',*,*,#3472,.F.);
#4690=ORIENTED_EDGE('',*,*,#3473,.F.);
#4691=ORIENTED_EDGE('',*,*,#3451,.F.);
#4692=ORIENTED_EDGE('',*,*,#3471,.F.);
#4693=ORIENTED_EDGE('',*,*,#3473,.T.);
#4694=ORIENTED_EDGE('',*,*,#3474,.T.);
#4695=ORIENTED_EDGE('',*,*,#3475,.T.);
#4696=ORIENTED_EDGE('',*,*,#3452,.T.);
#4697=ORIENTED_EDGE('',*,*,#3476,.F.);
#4698=ORIENTED_EDGE('',*,*,#3477,.F.);
#4699=ORIENTED_EDGE('',*,*,#3456,.F.);
#4700=ORIENTED_EDGE('',*,*,#3453,.F.);
#4701=ORIENTED_EDGE('',*,*,#3475,.F.);
#4702=ORIENTED_EDGE('',*,*,#3478,.F.);
#4703=ORIENTED_EDGE('',*,*,#3477,.T.);
#4704=ORIENTED_EDGE('',*,*,#3479,.T.);
#4705=ORIENTED_EDGE('',*,*,#3480,.T.);
#4706=ORIENTED_EDGE('',*,*,#3457,.T.);
#4707=ORIENTED_EDGE('',*,*,#3481,.F.);
#4708=ORIENTED_EDGE('',*,*,#3482,.F.);
#4709=ORIENTED_EDGE('',*,*,#3458,.F.);
#4710=ORIENTED_EDGE('',*,*,#3480,.F.);
#4711=ORIENTED_EDGE('',*,*,#3482,.T.);
#4712=ORIENTED_EDGE('',*,*,#3483,.T.);
#4713=ORIENTED_EDGE('',*,*,#3484,.T.);
#4714=ORIENTED_EDGE('',*,*,#3459,.T.);
#4715=ORIENTED_EDGE('',*,*,#3485,.F.);
#4716=ORIENTED_EDGE('',*,*,#3486,.F.);
#4717=ORIENTED_EDGE('',*,*,#3460,.F.);
#4718=ORIENTED_EDGE('',*,*,#3484,.F.);
#4719=ORIENTED_EDGE('',*,*,#3486,.T.);
#4720=ORIENTED_EDGE('',*,*,#3487,.T.);
#4721=ORIENTED_EDGE('',*,*,#3488,.T.);
#4722=ORIENTED_EDGE('',*,*,#3461,.T.);
#4723=ORIENTED_EDGE('',*,*,#3462,.F.);
#4724=ORIENTED_EDGE('',*,*,#3488,.F.);
#4725=ORIENTED_EDGE('',*,*,#3489,.F.);
#4726=ORIENTED_EDGE('',*,*,#3490,.F.);
#4727=ORIENTED_EDGE('',*,*,#3491,.F.);
#4728=ORIENTED_EDGE('',*,*,#3492,.T.);
#4729=ORIENTED_EDGE('',*,*,#3478,.T.);
#4730=ORIENTED_EDGE('',*,*,#3474,.F.);
#4731=ORIENTED_EDGE('',*,*,#3472,.T.);
#4732=ORIENTED_EDGE('',*,*,#3470,.F.);
#4733=ORIENTED_EDGE('',*,*,#3468,.T.);
#4734=ORIENTED_EDGE('',*,*,#3466,.F.);
#4735=ORIENTED_EDGE('',*,*,#3444,.T.);
#4736=ORIENTED_EDGE('',*,*,#3493,.F.);
#4737=ORIENTED_EDGE('',*,*,#3494,.T.);
#4738=ORIENTED_EDGE('',*,*,#3495,.F.);
#4739=ORIENTED_EDGE('',*,*,#3489,.T.);
#4740=ORIENTED_EDGE('',*,*,#3487,.F.);
#4741=ORIENTED_EDGE('',*,*,#3485,.T.);
#4742=ORIENTED_EDGE('',*,*,#3483,.F.);
#4743=ORIENTED_EDGE('',*,*,#3481,.T.);
#4744=ORIENTED_EDGE('',*,*,#3479,.F.);
#4745=ORIENTED_EDGE('',*,*,#3476,.T.);
#4746=ORIENTED_EDGE('',*,*,#3492,.F.);
#4747=ORIENTED_EDGE('',*,*,#3447,.T.);
#4748=ORIENTED_EDGE('',*,*,#3465,.T.);
#4749=ORIENTED_EDGE('',*,*,#3496,.T.);
#4750=ORIENTED_EDGE('',*,*,#3493,.T.);
#4751=ORIENTED_EDGE('',*,*,#3464,.F.);
#4752=ORIENTED_EDGE('',*,*,#3497,.F.);
#4753=ORIENTED_EDGE('',*,*,#3494,.F.);
#4754=ORIENTED_EDGE('',*,*,#3496,.F.);
#4755=ORIENTED_EDGE('',*,*,#3455,.T.);
#4756=ORIENTED_EDGE('',*,*,#3491,.T.);
#4757=ORIENTED_EDGE('',*,*,#3490,.T.);
#4758=ORIENTED_EDGE('',*,*,#3495,.T.);
#4759=ORIENTED_EDGE('',*,*,#3497,.T.);
#4760=ORIENTED_EDGE('',*,*,#3463,.T.);
#4761=ORIENTED_EDGE('',*,*,#3498,.F.);
#4762=ORIENTED_EDGE('',*,*,#3499,.T.);
#4763=ORIENTED_EDGE('',*,*,#3500,.F.);
#4764=ORIENTED_EDGE('',*,*,#3501,.T.);
#4765=ORIENTED_EDGE('',*,*,#3498,.T.);
#4766=ORIENTED_EDGE('',*,*,#3501,.F.);
#4767=ORIENTED_EDGE('',*,*,#3500,.T.);
#4768=ORIENTED_EDGE('',*,*,#3502,.F.);
#4769=ORIENTED_EDGE('',*,*,#3502,.T.);
#4770=ORIENTED_EDGE('',*,*,#3503,.T.);
#4771=ORIENTED_EDGE('',*,*,#3499,.F.);
#4772=ORIENTED_EDGE('',*,*,#3503,.F.);
#4773=ORIENTED_EDGE('',*,*,#3504,.F.);
#4774=ORIENTED_EDGE('',*,*,#3505,.T.);
#4775=ORIENTED_EDGE('',*,*,#3506,.F.);
#4776=ORIENTED_EDGE('',*,*,#3507,.T.);
#4777=ORIENTED_EDGE('',*,*,#3504,.T.);
#4778=ORIENTED_EDGE('',*,*,#3507,.F.);
#4779=ORIENTED_EDGE('',*,*,#3506,.T.);
#4780=ORIENTED_EDGE('',*,*,#3508,.F.);
#4781=ORIENTED_EDGE('',*,*,#3508,.T.);
#4782=ORIENTED_EDGE('',*,*,#3509,.T.);
#4783=ORIENTED_EDGE('',*,*,#3505,.F.);
#4784=ORIENTED_EDGE('',*,*,#3509,.F.);
#4785=ORIENTED_EDGE('',*,*,#3510,.F.);
#4786=ORIENTED_EDGE('',*,*,#3511,.F.);
#4787=ORIENTED_EDGE('',*,*,#3512,.T.);
#4788=ORIENTED_EDGE('',*,*,#3510,.T.);
#4789=ORIENTED_EDGE('',*,*,#3512,.F.);
#4790=ORIENTED_EDGE('',*,*,#3513,.F.);
#4791=ORIENTED_EDGE('',*,*,#3514,.T.);
#4792=ORIENTED_EDGE('',*,*,#3511,.T.);
#4793=ORIENTED_EDGE('',*,*,#3514,.F.);
#4794=ORIENTED_EDGE('',*,*,#3515,.F.);
#4795=ORIENTED_EDGE('',*,*,#3516,.T.);
#4796=ORIENTED_EDGE('',*,*,#3513,.T.);
#4797=ORIENTED_EDGE('',*,*,#3516,.F.);
#4798=ORIENTED_EDGE('',*,*,#3515,.T.);
#4799=ORIENTED_EDGE('',*,*,#3517,.F.);
#4800=ORIENTED_EDGE('',*,*,#3518,.F.);
#4801=ORIENTED_EDGE('',*,*,#3519,.T.);
#4802=ORIENTED_EDGE('',*,*,#3517,.T.);
#4803=ORIENTED_EDGE('',*,*,#3519,.F.);
#4804=ORIENTED_EDGE('',*,*,#3520,.F.);
#4805=ORIENTED_EDGE('',*,*,#3521,.T.);
#4806=ORIENTED_EDGE('',*,*,#3518,.T.);
#4807=ORIENTED_EDGE('',*,*,#3521,.F.);
#4808=ORIENTED_EDGE('',*,*,#3522,.F.);
#4809=ORIENTED_EDGE('',*,*,#3523,.T.);
#4810=ORIENTED_EDGE('',*,*,#3520,.T.);
#4811=ORIENTED_EDGE('',*,*,#3523,.F.);
#4812=ORIENTED_EDGE('',*,*,#3522,.T.);
#4813=ORIENTED_EDGE('',*,*,#3524,.T.);
#4814=ORIENTED_EDGE('',*,*,#3525,.T.);
#4815=ORIENTED_EDGE('',*,*,#3526,.T.);
#4816=ORIENTED_EDGE('',*,*,#3527,.F.);
#4817=ORIENTED_EDGE('',*,*,#3528,.T.);
#4818=ORIENTED_EDGE('',*,*,#3529,.T.);
#4819=ORIENTED_EDGE('',*,*,#3530,.T.);
#4820=ORIENTED_EDGE('',*,*,#3525,.F.);
#4821=ORIENTED_EDGE('',*,*,#3531,.T.);
#4822=ORIENTED_EDGE('',*,*,#3532,.T.);
#4823=ORIENTED_EDGE('',*,*,#3533,.T.);
#4824=ORIENTED_EDGE('',*,*,#3529,.F.);
#4825=ORIENTED_EDGE('',*,*,#3534,.T.);
#4826=ORIENTED_EDGE('',*,*,#3535,.T.);
#4827=ORIENTED_EDGE('',*,*,#3536,.T.);
#4828=ORIENTED_EDGE('',*,*,#3532,.F.);
#4829=ORIENTED_EDGE('',*,*,#3537,.T.);
#4830=ORIENTED_EDGE('',*,*,#3538,.T.);
#4831=ORIENTED_EDGE('',*,*,#3539,.T.);
#4832=ORIENTED_EDGE('',*,*,#3535,.F.);
#4833=ORIENTED_EDGE('',*,*,#3540,.T.);
#4834=ORIENTED_EDGE('',*,*,#3527,.T.);
#4835=ORIENTED_EDGE('',*,*,#3541,.T.);
#4836=ORIENTED_EDGE('',*,*,#3538,.F.);
#4837=ORIENTED_EDGE('',*,*,#3540,.F.);
#4838=ORIENTED_EDGE('',*,*,#3537,.F.);
#4839=ORIENTED_EDGE('',*,*,#3534,.F.);
#4840=ORIENTED_EDGE('',*,*,#3531,.F.);
#4841=ORIENTED_EDGE('',*,*,#3528,.F.);
#4842=ORIENTED_EDGE('',*,*,#3524,.F.);
#4843=ORIENTED_EDGE('',*,*,#3541,.F.);
#4844=ORIENTED_EDGE('',*,*,#3526,.F.);
#4845=ORIENTED_EDGE('',*,*,#3530,.F.);
#4846=ORIENTED_EDGE('',*,*,#3533,.F.);
#4847=ORIENTED_EDGE('',*,*,#3536,.F.);
#4848=ORIENTED_EDGE('',*,*,#3539,.F.);
#4849=ORIENTED_EDGE('',*,*,#3542,.F.);
#4850=ORIENTED_EDGE('',*,*,#3543,.T.);
#4851=ORIENTED_EDGE('',*,*,#3544,.F.);
#4852=ORIENTED_EDGE('',*,*,#3543,.F.);
#4853=ORIENTED_EDGE('',*,*,#3542,.T.);
#4854=ORIENTED_EDGE('',*,*,#3545,.F.);
#4855=ORIENTED_EDGE('',*,*,#3545,.T.);
#4856=ORIENTED_EDGE('',*,*,#3546,.T.);
#4857=ORIENTED_EDGE('',*,*,#3547,.T.);
#4858=ORIENTED_EDGE('',*,*,#3546,.F.);
#4859=ORIENTED_EDGE('',*,*,#3548,.F.);
#4860=ORIENTED_EDGE('',*,*,#3549,.T.);
#4861=ORIENTED_EDGE('',*,*,#3550,.T.);
#4862=ORIENTED_EDGE('',*,*,#3549,.F.);
#4863=ORIENTED_EDGE('',*,*,#3548,.T.);
#4864=ORIENTED_EDGE('',*,*,#3544,.T.);
#4865=ORIENTED_EDGE('',*,*,#3550,.F.);
#4866=ORIENTED_EDGE('',*,*,#3547,.F.);
#4867=ORIENTED_EDGE('',*,*,#3551,.F.);
#4868=ORIENTED_EDGE('',*,*,#3552,.T.);
#4869=ORIENTED_EDGE('',*,*,#3553,.T.);
#4870=ORIENTED_EDGE('',*,*,#3552,.F.);
#4871=ORIENTED_EDGE('',*,*,#3554,.F.);
#4872=ORIENTED_EDGE('',*,*,#3555,.T.);
#4873=ORIENTED_EDGE('',*,*,#3556,.T.);
#4874=ORIENTED_EDGE('',*,*,#3555,.F.);
#4875=ORIENTED_EDGE('',*,*,#3554,.T.);
#4876=ORIENTED_EDGE('',*,*,#3551,.T.);
#4877=ORIENTED_EDGE('',*,*,#3556,.F.);
#4878=ORIENTED_EDGE('',*,*,#3553,.F.);
#4879=CYLINDRICAL_SURFACE('',#5700,0.25);
#4880=CYLINDRICAL_SURFACE('',#5703,0.25);
#4881=CYLINDRICAL_SURFACE('',#5706,0.25);
#4882=CYLINDRICAL_SURFACE('',#5709,0.25);
#4883=CYLINDRICAL_SURFACE('',#5733,0.165);
#4884=CYLINDRICAL_SURFACE('',#5736,0.165);
#4885=CYLINDRICAL_SURFACE('',#5739,0.165);
#4886=CYLINDRICAL_SURFACE('',#5742,0.165);
#4887=CYLINDRICAL_SURFACE('',#5745,0.33);
#4888=CYLINDRICAL_SURFACE('',#5748,0.33);
#4889=CYLINDRICAL_SURFACE('',#5751,0.33);
#4890=CYLINDRICAL_SURFACE('',#5754,0.33);
#4891=CYLINDRICAL_SURFACE('',#5757,1.6);
#4892=CYLINDRICAL_SURFACE('',#5771,1.2);
#4893=CYLINDRICAL_SURFACE('',#5774,1.59);
#4894=CYLINDRICAL_SURFACE('',#5780,0.225);
#4895=CYLINDRICAL_SURFACE('',#5783,0.225);
#4896=CYLINDRICAL_SURFACE('',#5786,0.225);
#4897=CYLINDRICAL_SURFACE('',#5789,0.225);
#4898=CYLINDRICAL_SURFACE('',#5792,1.59);
#4899=CYLINDRICAL_SURFACE('',#5797,1.2);
#4900=CYLINDRICAL_SURFACE('',#5799,2.4);
#4901=CYLINDRICAL_SURFACE('',#5805,0.225);
#4902=CYLINDRICAL_SURFACE('',#5808,0.225);
#4903=CYLINDRICAL_SURFACE('',#5811,0.225);
#4904=CYLINDRICAL_SURFACE('',#5814,0.225);
#4905=CYLINDRICAL_SURFACE('',#5817,1.59);
#4906=CYLINDRICAL_SURFACE('',#5822,1.2);
#4907=CYLINDRICAL_SURFACE('',#5824,2.4);
#4908=CYLINDRICAL_SURFACE('',#5830,0.32);
#4909=CYLINDRICAL_SURFACE('',#5833,0.6);
#4910=CYLINDRICAL_SURFACE('',#5853,0.5);
#4911=CYLINDRICAL_SURFACE('',#5861,0.2942);
#4912=CYLINDRICAL_SURFACE('',#5870,1.070235);
#4913=CYLINDRICAL_SURFACE('',#5872,0.6);
#4914=CYLINDRICAL_SURFACE('',#5878,1.070235);
#4915=CYLINDRICAL_SURFACE('',#5890,1.129765);
#4916=CYLINDRICAL_SURFACE('',#5897,1.6);
#4917=CYLINDRICAL_SURFACE('',#5902,1.129765);
#4918=CYLINDRICAL_SURFACE('',#5922,1.123812);
#4919=CYLINDRICAL_SURFACE('',#5958,1.076188);
#4920=CYLINDRICAL_SURFACE('',#5972,1.119765);
#4921=CYLINDRICAL_SURFACE('',#5976,1.085235);
#4922=CYLINDRICAL_SURFACE('',#5980,1.119765);
#4923=CYLINDRICAL_SURFACE('',#5984,1.085235);
#4924=CYLINDRICAL_SURFACE('',#6005,0.8);
#4925=CYLINDRICAL_SURFACE('',#6006,0.6);
#4926=CYLINDRICAL_SURFACE('',#6008,0.6);
#4927=CYLINDRICAL_SURFACE('',#6013,0.165);
#4928=CYLINDRICAL_SURFACE('',#6016,0.165);
#4929=CYLINDRICAL_SURFACE('',#6021,0.21);
#4930=CYLINDRICAL_SURFACE('',#6031,0.6);
#4931=CYLINDRICAL_SURFACE('',#6043,7.25);
#4932=CYLINDRICAL_SURFACE('',#6047,7.25);
#4933=CYLINDRICAL_SURFACE('',#6057,7.25);
#4934=CYLINDRICAL_SURFACE('',#6058,8.);
#4935=CYLINDRICAL_SURFACE('',#6059,1.5);
#4936=CYLINDRICAL_SURFACE('',#6063,0.605);
#4937=CYLINDRICAL_SURFACE('',#6066,0.8);
#4938=CYLINDRICAL_SURFACE('',#6074,0.21);
#4939=CYLINDRICAL_SURFACE('',#6078,0.605);
#4940=CYLINDRICAL_SURFACE('',#6081,1.1);
#4941=CYLINDRICAL_SURFACE('',#6087,0.165);
#4942=CYLINDRICAL_SURFACE('',#6091,0.225);
#4943=CYLINDRICAL_SURFACE('',#6094,0.225);
#4944=CYLINDRICAL_SURFACE('',#6100,1.7);
#4945=CYLINDRICAL_SURFACE('',#6105,0.7);
#4946=CYLINDRICAL_SURFACE('',#6106,0.5);
#4947=CYLINDRICAL_SURFACE('',#6111,0.505);
#4948=CYLINDRICAL_SURFACE('',#6114,0.7);
#4949=CYLINDRICAL_SURFACE('',#6120,0.225);
#4950=CYLINDRICAL_SURFACE('',#6123,0.9);
#4951=CYLINDRICAL_SURFACE('',#6137,0.2);
#4952=CYLINDRICAL_SURFACE('',#6148,0.2);
#4953=CYLINDRICAL_SURFACE('',#6163,0.24505);
#4954=CYLINDRICAL_SURFACE('',#6183,0.35);
#4955=CYLINDRICAL_SURFACE('',#6191,0.1954);
#4956=CYLINDRICAL_SURFACE('',#6200,0.976185);
#4957=CYLINDRICAL_SURFACE('',#6202,0.5);
#4958=CYLINDRICAL_SURFACE('',#6208,0.976185);
#4959=CYLINDRICAL_SURFACE('',#6220,1.023815);
#4960=CYLINDRICAL_SURFACE('',#6227,1.5);
#4961=CYLINDRICAL_SURFACE('',#6232,1.023815);
#4962=CYLINDRICAL_SURFACE('',#6254,1.019052);
#4963=CYLINDRICAL_SURFACE('',#6294,0.980948);
#4964=CYLINDRICAL_SURFACE('',#6308,1.013815);
#4965=CYLINDRICAL_SURFACE('',#6312,0.991185);
#4966=CYLINDRICAL_SURFACE('',#6316,1.013815);
#4967=CYLINDRICAL_SURFACE('',#6320,0.991185);
#4968=CYLINDRICAL_SURFACE('',#6331,0.35);
#4969=CYLINDRICAL_SURFACE('',#6339,0.1954);
#4970=CYLINDRICAL_SURFACE('',#6393,1.5);
#4971=CYLINDRICAL_SURFACE('',#6398,0.91);
#4972=CYLINDRICAL_SURFACE('',#6400,1.8);
#4973=CYLINDRICAL_SURFACE('',#6406,0.91);
#4974=CYLINDRICAL_SURFACE('',#6409,1.8);
#4975=ADVANCED_FACE('',(#763),#4879,.F.);
#4976=ADVANCED_FACE('',(#764),#4880,.F.);
#4977=ADVANCED_FACE('',(#765),#4881,.F.);
#4978=ADVANCED_FACE('',(#766),#4882,.F.);
#4979=ADVANCED_FACE('',(#767),#598,.T.);
#4980=ADVANCED_FACE('',(#768),#599,.T.);
#4981=ADVANCED_FACE('',(#769),#600,.T.);
#4982=ADVANCED_FACE('',(#770),#601,.T.);
#4983=ADVANCED_FACE('',(#771,#486,#487,#488,#489),#602,.T.);
#4984=ADVANCED_FACE('',(#772,#490,#491,#492,#493),#603,.F.);
#4985=ADVANCED_FACE('',(#773),#604,.T.);
#4986=ADVANCED_FACE('',(#774),#605,.T.);
#4987=ADVANCED_FACE('',(#775),#606,.T.);
#4988=ADVANCED_FACE('',(#776),#607,.T.);
#4989=ADVANCED_FACE('',(#777),#608,.T.);
#4990=ADVANCED_FACE('',(#778),#609,.F.);
#4991=ADVANCED_FACE('',(#779),#610,.T.);
#4992=ADVANCED_FACE('',(#780),#611,.T.);
#4993=ADVANCED_FACE('',(#781),#612,.T.);
#4994=ADVANCED_FACE('',(#782),#613,.T.);
#4995=ADVANCED_FACE('',(#783),#614,.T.);
#4996=ADVANCED_FACE('',(#784),#615,.F.);
#4997=ADVANCED_FACE('',(#785),#4883,.F.);
#4998=ADVANCED_FACE('',(#786),#4884,.F.);
#4999=ADVANCED_FACE('',(#787),#4885,.F.);
#5000=ADVANCED_FACE('',(#788),#4886,.F.);
#5001=ADVANCED_FACE('',(#789),#4887,.F.);
#5002=ADVANCED_FACE('',(#790),#4888,.F.);
#5003=ADVANCED_FACE('',(#791),#4889,.F.);
#5004=ADVANCED_FACE('',(#792),#4890,.F.);
#5005=ADVANCED_FACE('',(#793),#4891,.F.);
#5006=ADVANCED_FACE('',(#794,#494,#495),#616,.T.);
#5007=ADVANCED_FACE('',(#795,#496,#497),#617,.T.);
#5008=ADVANCED_FACE('',(#796),#618,.T.);
#5009=ADVANCED_FACE('',(#797),#619,.T.);
#5010=ADVANCED_FACE('',(#798,#498,#499,#500,#501,#502),#620,.T.);
#5011=ADVANCED_FACE('',(#799),#621,.T.);
#5012=ADVANCED_FACE('',(#800,#503,#504,#505,#506,#507),#622,.T.);
#5013=ADVANCED_FACE('',(#801),#623,.T.);
#5014=ADVANCED_FACE('',(#802),#624,.T.);
#5015=ADVANCED_FACE('',(#803,#508,#509,#510,#511),#625,.F.);
#5016=ADVANCED_FACE('',(#804),#4892,.F.);
#5017=ADVANCED_FACE('',(#805),#4893,.T.);
#5018=ADVANCED_FACE('',(#806,#512),#626,.T.);
#5019=ADVANCED_FACE('',(#807,#513),#627,.F.);
#5020=ADVANCED_FACE('',(#808),#4894,.F.);
#5021=ADVANCED_FACE('',(#809),#4895,.F.);
#5022=ADVANCED_FACE('',(#810),#4896,.F.);
#5023=ADVANCED_FACE('',(#811),#4897,.F.);
#5024=ADVANCED_FACE('',(#812),#4898,.T.);
#5025=ADVANCED_FACE('',(#813,#514),#628,.T.);
#5026=ADVANCED_FACE('',(#814),#4899,.F.);
#5027=ADVANCED_FACE('',(#815),#4900,.T.);
#5028=ADVANCED_FACE('',(#816,#515,#516,#517,#518,#519),#629,.T.);
#5029=ADVANCED_FACE('',(#817,#520,#521,#522,#523,#524),#630,.F.);
#5030=ADVANCED_FACE('',(#818),#4901,.F.);
#5031=ADVANCED_FACE('',(#819),#4902,.F.);
#5032=ADVANCED_FACE('',(#820),#4903,.F.);
#5033=ADVANCED_FACE('',(#821),#4904,.F.);
#5034=ADVANCED_FACE('',(#822),#4905,.T.);
#5035=ADVANCED_FACE('',(#823,#525),#631,.F.);
#5036=ADVANCED_FACE('',(#824),#4906,.F.);
#5037=ADVANCED_FACE('',(#825),#4907,.T.);
#5038=ADVANCED_FACE('',(#826,#526,#527,#528,#529,#530),#632,.T.);
#5039=ADVANCED_FACE('',(#827,#531,#532,#533,#534,#535),#633,.F.);
#5040=ADVANCED_FACE('',(#828),#4908,.F.);
#5041=ADVANCED_FACE('',(#829),#4909,.T.);
#5042=ADVANCED_FACE('',(#830,#536),#634,.T.);
#5043=ADVANCED_FACE('',(#831,#537),#635,.F.);
#5044=ADVANCED_FACE('',(#832),#636,.F.);
#5045=ADVANCED_FACE('',(#833),#637,.F.);
#5046=ADVANCED_FACE('',(#834),#638,.F.);
#5047=ADVANCED_FACE('',(#835),#639,.F.);
#5048=ADVANCED_FACE('',(#836),#640,.F.);
#5049=ADVANCED_FACE('',(#837),#641,.F.);
#5050=ADVANCED_FACE('',(#838),#642,.F.);
#5051=ADVANCED_FACE('',(#839),#643,.F.);
#5052=ADVANCED_FACE('',(#840),#644,.F.);
#5053=ADVANCED_FACE('',(#841),#645,.T.);
#5054=ADVANCED_FACE('',(#842),#301,.T.);
#5055=ADVANCED_FACE('',(#843),#4910,.T.);
#5056=ADVANCED_FACE('',(#844),#302,.T.);
#5057=ADVANCED_FACE('',(#845,#538),#646,.T.);
#5058=ADVANCED_FACE('',(#846),#303,.T.);
#5059=ADVANCED_FACE('',(#847),#4911,.T.);
#5060=ADVANCED_FACE('',(#848),#297,.F.);
#5061=ADVANCED_FACE('',(#849),#4912,.T.);
#5062=ADVANCED_FACE('',(#850),#4913,.F.);
#5063=ADVANCED_FACE('',(#851),#304,.F.);
#5064=ADVANCED_FACE('',(#852,#539),#647,.T.);
#5065=ADVANCED_FACE('',(#853),#4914,.T.);
#5066=ADVANCED_FACE('',(#854,#540),#648,.T.);
#5067=ADVANCED_FACE('',(#855),#305,.F.);
#5068=ADVANCED_FACE('',(#856),#298,.F.);
#5069=ADVANCED_FACE('',(#857),#4915,.F.);
#5070=ADVANCED_FACE('',(#858,#541),#649,.T.);
#5071=ADVANCED_FACE('',(#859),#306,.T.);
#5072=ADVANCED_FACE('',(#860),#4916,.T.);
#5073=ADVANCED_FACE('',(#861),#307,.T.);
#5074=ADVANCED_FACE('',(#862,#542),#650,.T.);
#5075=ADVANCED_FACE('',(#863),#4917,.F.);
#5076=ADVANCED_FACE('',(#864),#267,.T.);
#5077=ADVANCED_FACE('',(#865),#268,.T.);
#5078=ADVANCED_FACE('',(#866),#269,.T.);
#5079=ADVANCED_FACE('',(#867),#270,.T.);
#5080=ADVANCED_FACE('',(#868),#271,.T.);
#5081=ADVANCED_FACE('',(#869),#272,.T.);
#5082=ADVANCED_FACE('',(#870),#273,.T.);
#5083=ADVANCED_FACE('',(#871),#274,.F.);
#5084=ADVANCED_FACE('',(#872),#4918,.T.);
#5085=ADVANCED_FACE('',(#873),#651,.T.);
#5086=ADVANCED_FACE('',(#874),#275,.F.);
#5087=ADVANCED_FACE('',(#875),#652,.T.);
#5088=ADVANCED_FACE('',(#876),#276,.F.);
#5089=ADVANCED_FACE('',(#877),#653,.T.);
#5090=ADVANCED_FACE('',(#878),#277,.F.);
#5091=ADVANCED_FACE('',(#879),#654,.T.);
#5092=ADVANCED_FACE('',(#880),#278,.F.);
#5093=ADVANCED_FACE('',(#881),#655,.T.);
#5094=ADVANCED_FACE('',(#882),#279,.F.);
#5095=ADVANCED_FACE('',(#883),#4919,.F.);
#5096=ADVANCED_FACE('',(#884),#656,.T.);
#5097=ADVANCED_FACE('',(#885),#280,.F.);
#5098=ADVANCED_FACE('',(#886,#543),#657,.T.);
#5099=ADVANCED_FACE('',(#887),#658,.T.);
#5100=ADVANCED_FACE('',(#888,#544),#659,.T.);
#5101=ADVANCED_FACE('',(#889),#4920,.T.);
#5102=ADVANCED_FACE('',(#890,#545),#660,.T.);
#5103=ADVANCED_FACE('',(#891),#4921,.F.);
#5104=ADVANCED_FACE('',(#892,#546),#661,.T.);
#5105=ADVANCED_FACE('',(#893),#4922,.T.);
#5106=ADVANCED_FACE('',(#894,#547),#662,.T.);
#5107=ADVANCED_FACE('',(#895),#4923,.F.);
#5108=ADVANCED_FACE('',(#896),#663,.F.);
#5109=ADVANCED_FACE('',(#897),#664,.T.);
#5110=ADVANCED_FACE('',(#898),#665,.F.);
#5111=ADVANCED_FACE('',(#899),#666,.F.);
#5112=ADVANCED_FACE('',(#900),#667,.F.);
#5113=ADVANCED_FACE('',(#901,#548),#668,.T.);
#5114=ADVANCED_FACE('',(#902,#549),#669,.F.);
#5115=ADVANCED_FACE('',(#903),#4924,.T.);
#5116=ADVANCED_FACE('',(#904,#550),#4925,.T.);
#5117=ADVANCED_FACE('',(#905),#4926,.T.);
#5118=ADVANCED_FACE('',(#906),#670,.T.);
#5119=ADVANCED_FACE('',(#907),#671,.F.);
#5120=ADVANCED_FACE('',(#908),#4927,.F.);
#5121=ADVANCED_FACE('',(#909),#4928,.F.);
#5122=ADVANCED_FACE('',(#910),#672,.T.);
#5123=ADVANCED_FACE('',(#911),#4929,.F.);
#5124=ADVANCED_FACE('',(#912),#673,.T.);
#5125=ADVANCED_FACE('',(#913),#674,.F.);
#5126=ADVANCED_FACE('',(#914),#675,.F.);
#5127=ADVANCED_FACE('',(#915),#676,.F.);
#5128=ADVANCED_FACE('',(#916,#551),#677,.T.);
#5129=ADVANCED_FACE('',(#917,#552),#4930,.F.);
#5130=ADVANCED_FACE('',(#918),#678,.T.);
#5131=ADVANCED_FACE('',(#919),#679,.T.);
#5132=ADVANCED_FACE('',(#920,#553,#554,#555),#680,.F.);
#5133=ADVANCED_FACE('',(#921),#4931,.F.);
#5134=ADVANCED_FACE('',(#922),#681,.T.);
#5135=ADVANCED_FACE('',(#923),#682,.T.);
#5136=ADVANCED_FACE('',(#924),#4932,.F.);
#5137=ADVANCED_FACE('',(#925),#683,.T.);
#5138=ADVANCED_FACE('',(#926),#684,.T.);
#5139=ADVANCED_FACE('',(#927,#556,#557,#558),#685,.T.);
#5140=ADVANCED_FACE('',(#928),#4933,.F.);
#5141=ADVANCED_FACE('',(#929),#4934,.T.);
#5142=ADVANCED_FACE('',(#930,#559,#560,#561,#562),#4935,.T.);
#5143=ADVANCED_FACE('',(#931,#563),#686,.F.);
#5144=ADVANCED_FACE('',(#932),#4936,.F.);
#5145=ADVANCED_FACE('',(#933),#4937,.T.);
#5146=ADVANCED_FACE('',(#934,#564),#687,.T.);
#5147=ADVANCED_FACE('',(#935,#565),#688,.F.);
#5148=ADVANCED_FACE('',(#936),#689,.T.);
#5149=ADVANCED_FACE('',(#937),#4938,.F.);
#5150=ADVANCED_FACE('',(#938),#690,.T.);
#5151=ADVANCED_FACE('',(#939,#566),#4939,.F.);
#5152=ADVANCED_FACE('',(#940,#567),#4940,.T.);
#5153=ADVANCED_FACE('',(#941,#568),#691,.T.);
#5154=ADVANCED_FACE('',(#942,#569),#692,.F.);
#5155=ADVANCED_FACE('',(#943),#4941,.F.);
#5156=ADVANCED_FACE('',(#944),#693,.F.);
#5157=ADVANCED_FACE('',(#945),#4942,.F.);
#5158=ADVANCED_FACE('',(#946),#4943,.F.);
#5159=ADVANCED_FACE('',(#947,#570,#571,#572),#694,.F.);
#5160=ADVANCED_FACE('',(#948),#4944,.T.);
#5161=ADVANCED_FACE('',(#949,#573),#695,.F.);
#5162=ADVANCED_FACE('',(#950),#4945,.T.);
#5163=ADVANCED_FACE('',(#951),#4946,.T.);
#5164=ADVANCED_FACE('',(#952,#574,#575),#696,.T.);
#5165=ADVANCED_FACE('',(#953,#576),#697,.F.);
#5166=ADVANCED_FACE('',(#954),#4947,.F.);
#5167=ADVANCED_FACE('',(#955),#4948,.T.);
#5168=ADVANCED_FACE('',(#956,#577),#698,.T.);
#5169=ADVANCED_FACE('',(#957,#578),#699,.F.);
#5170=ADVANCED_FACE('',(#958),#4949,.F.);
#5171=ADVANCED_FACE('',(#959),#4950,.T.);
#5172=ADVANCED_FACE('',(#960,#579),#700,.T.);
#5173=ADVANCED_FACE('',(#961,#580),#701,.F.);
#5174=ADVANCED_FACE('',(#962),#702,.T.);
#5175=ADVANCED_FACE('',(#963),#308,.T.);
#5176=ADVANCED_FACE('',(#964),#703,.T.);
#5177=ADVANCED_FACE('',(#965),#309,.T.);
#5178=ADVANCED_FACE('',(#966),#4951,.T.);
#5179=ADVANCED_FACE('',(#967),#704,.T.);
#5180=ADVANCED_FACE('',(#968),#705,.T.);
#5181=ADVANCED_FACE('',(#969),#706,.T.);
#5182=ADVANCED_FACE('',(#970),#310,.T.);
#5183=ADVANCED_FACE('',(#971),#707,.T.);
#5184=ADVANCED_FACE('',(#972),#311,.T.);
#5185=ADVANCED_FACE('',(#973),#4952,.T.);
#5186=ADVANCED_FACE('',(#974),#708,.F.);
#5187=ADVANCED_FACE('',(#975),#709,.T.);
#5188=ADVANCED_FACE('',(#976),#710,.F.);
#5189=ADVANCED_FACE('',(#977),#711,.F.);
#5190=ADVANCED_FACE('',(#978),#712,.F.);
#5191=ADVANCED_FACE('',(#979),#713,.F.);
#5192=ADVANCED_FACE('',(#980),#714,.F.);
#5193=ADVANCED_FACE('',(#981),#715,.F.);
#5194=ADVANCED_FACE('',(#982),#716,.F.);
#5195=ADVANCED_FACE('',(#983,#581),#717,.T.);
#5196=ADVANCED_FACE('',(#984),#312,.T.);
#5197=ADVANCED_FACE('',(#985),#4953,.T.);
#5198=ADVANCED_FACE('',(#986),#313,.T.);
#5199=ADVANCED_FACE('',(#987),#718,.T.);
#5200=ADVANCED_FACE('',(#988),#719,.F.);
#5201=ADVANCED_FACE('',(#989),#720,.F.);
#5202=ADVANCED_FACE('',(#990),#721,.F.);
#5203=ADVANCED_FACE('',(#991),#722,.F.);
#5204=ADVANCED_FACE('',(#992),#723,.F.);
#5205=ADVANCED_FACE('',(#993),#724,.F.);
#5206=ADVANCED_FACE('',(#994),#725,.F.);
#5207=ADVANCED_FACE('',(#995),#726,.F.);
#5208=ADVANCED_FACE('',(#996),#727,.F.);
#5209=ADVANCED_FACE('',(#997),#728,.T.);
#5210=ADVANCED_FACE('',(#998),#314,.T.);
#5211=ADVANCED_FACE('',(#999),#4954,.T.);
#5212=ADVANCED_FACE('',(#1000),#315,.T.);
#5213=ADVANCED_FACE('',(#1001,#582),#729,.T.);
#5214=ADVANCED_FACE('',(#1002),#316,.T.);
#5215=ADVANCED_FACE('',(#1003),#4955,.T.);
#5216=ADVANCED_FACE('',(#1004),#299,.F.);
#5217=ADVANCED_FACE('',(#1005),#4956,.T.);
#5218=ADVANCED_FACE('',(#1006),#4957,.F.);
#5219=ADVANCED_FACE('',(#1007),#317,.F.);
#5220=ADVANCED_FACE('',(#1008,#583),#730,.T.);
#5221=ADVANCED_FACE('',(#1009),#4958,.T.);
#5222=ADVANCED_FACE('',(#1010,#584),#731,.T.);
#5223=ADVANCED_FACE('',(#1011),#318,.F.);
#5224=ADVANCED_FACE('',(#1012),#300,.F.);
#5225=ADVANCED_FACE('',(#1013),#4959,.F.);
#5226=ADVANCED_FACE('',(#1014,#585),#732,.T.);
#5227=ADVANCED_FACE('',(#1015),#319,.T.);
#5228=ADVANCED_FACE('',(#1016),#4960,.T.);
#5229=ADVANCED_FACE('',(#1017),#320,.T.);
#5230=ADVANCED_FACE('',(#1018,#586),#733,.T.);
#5231=ADVANCED_FACE('',(#1019),#4961,.F.);
#5232=ADVANCED_FACE('',(#1020),#281,.T.);
#5233=ADVANCED_FACE('',(#1021),#282,.T.);
#5234=ADVANCED_FACE('',(#1022),#283,.T.);
#5235=ADVANCED_FACE('',(#1023),#284,.T.);
#5236=ADVANCED_FACE('',(#1024),#285,.T.);
#5237=ADVANCED_FACE('',(#1025),#286,.T.);
#5238=ADVANCED_FACE('',(#1026),#287,.T.);
#5239=ADVANCED_FACE('',(#1027),#288,.T.);
#5240=ADVANCED_FACE('',(#1028),#289,.F.);
#5241=ADVANCED_FACE('',(#1029),#4962,.T.);
#5242=ADVANCED_FACE('',(#1030),#734,.T.);
#5243=ADVANCED_FACE('',(#1031),#290,.F.);
#5244=ADVANCED_FACE('',(#1032),#735,.T.);
#5245=ADVANCED_FACE('',(#1033),#291,.F.);
#5246=ADVANCED_FACE('',(#1034),#736,.T.);
#5247=ADVANCED_FACE('',(#1035),#292,.F.);
#5248=ADVANCED_FACE('',(#1036),#737,.T.);
#5249=ADVANCED_FACE('',(#1037),#293,.F.);
#5250=ADVANCED_FACE('',(#1038),#738,.T.);
#5251=ADVANCED_FACE('',(#1039),#294,.F.);
#5252=ADVANCED_FACE('',(#1040),#739,.T.);
#5253=ADVANCED_FACE('',(#1041),#295,.F.);
#5254=ADVANCED_FACE('',(#1042),#4963,.F.);
#5255=ADVANCED_FACE('',(#1043),#740,.T.);
#5256=ADVANCED_FACE('',(#1044),#296,.F.);
#5257=ADVANCED_FACE('',(#1045,#587),#741,.T.);
#5258=ADVANCED_FACE('',(#1046),#742,.T.);
#5259=ADVANCED_FACE('',(#1047,#588),#743,.T.);
#5260=ADVANCED_FACE('',(#1048),#4964,.T.);
#5261=ADVANCED_FACE('',(#1049,#589),#744,.T.);
#5262=ADVANCED_FACE('',(#1050),#4965,.F.);
#5263=ADVANCED_FACE('',(#1051,#590),#745,.T.);
#5264=ADVANCED_FACE('',(#1052),#4966,.T.);
#5265=ADVANCED_FACE('',(#1053,#591),#746,.T.);
#5266=ADVANCED_FACE('',(#1054),#4967,.F.);
#5267=ADVANCED_FACE('',(#1055),#747,.T.);
#5268=ADVANCED_FACE('',(#1056),#321,.T.);
#5269=ADVANCED_FACE('',(#1057),#4968,.T.);
#5270=ADVANCED_FACE('',(#1058),#322,.T.);
#5271=ADVANCED_FACE('',(#1059,#592),#748,.T.);
#5272=ADVANCED_FACE('',(#1060),#323,.T.);
#5273=ADVANCED_FACE('',(#1061),#4969,.T.);
#5274=ADVANCED_FACE('',(#1062),#324,.T.);
#5275=ADVANCED_FACE('',(#1063),#749,.T.);
#5276=ADVANCED_FACE('',(#1064),#750,.F.);
#5277=ADVANCED_FACE('',(#1065),#751,.F.);
#5278=ADVANCED_FACE('',(#1066),#752,.F.);
#5279=ADVANCED_FACE('',(#1067),#753,.F.);
#5280=ADVANCED_FACE('',(#1068),#754,.F.);
#5281=ADVANCED_FACE('',(#1069),#755,.F.);
#5282=ADVANCED_FACE('',(#1070),#756,.F.);
#5283=ADVANCED_FACE('',(#1071),#757,.F.);
#5284=ADVANCED_FACE('',(#1072),#4970,.F.);
#5285=ADVANCED_FACE('',(#1073,#593),#758,.T.);
#5286=ADVANCED_FACE('',(#1074),#4971,.F.);
#5287=ADVANCED_FACE('',(#1075),#4972,.T.);
#5288=ADVANCED_FACE('',(#1076,#594),#759,.T.);
#5289=ADVANCED_FACE('',(#1077,#595),#760,.F.);
#5290=ADVANCED_FACE('',(#1078),#4973,.F.);
#5291=ADVANCED_FACE('',(#1079),#4974,.T.);
#5292=ADVANCED_FACE('',(#1080,#596),#761,.T.);
#5293=ADVANCED_FACE('',(#1081,#597),#762,.F.);
#5294=CLOSED_SHELL('',(#4975,#4976,#4977,#4978,#4979,#4980,#4981,#4982,
#4983,#4984));
#5295=CLOSED_SHELL('',(#4985,#4986,#4987,#4988,#4989,#4990));
#5296=CLOSED_SHELL('',(#4991,#4992,#4993,#4994,#4995,#4996));
#5297=CLOSED_SHELL('',(#4997,#4998,#4999,#5000,#5001,#5002,#5003,#5004,
#5005,#5006,#5007,#5008,#5009,#5010,#5011,#5012,#5013,#5014,#5015));
#5298=CLOSED_SHELL('',(#5016,#5017,#5018,#5019));
#5299=CLOSED_SHELL('',(#5020,#5021,#5022,#5023,#5024,#5025,#5026,#5027,
#5028,#5029));
#5300=CLOSED_SHELL('',(#5030,#5031,#5032,#5033,#5034,#5035,#5036,#5037,
#5038,#5039));
#5301=CLOSED_SHELL('',(#5040,#5041,#5042,#5043));
#5302=CLOSED_SHELL('',(#5044,#5045,#5046,#5047,#5048,#5049,#5050,#5051));
#5303=CLOSED_SHELL('',(#5052,#5053,#5054,#5055,#5056,#5057,#5058,#5059));
#5304=CLOSED_SHELL('',(#5060,#5061,#5062,#5063,#5064,#5065,#5066,#5067));
#5305=CLOSED_SHELL('',(#5068,#5069,#5070,#5071,#5072,#5073,#5074,#5075));
#5306=CLOSED_SHELL('',(#5076));
#5307=CLOSED_SHELL('',(#5077));
#5308=CLOSED_SHELL('',(#5078));
#5309=CLOSED_SHELL('',(#5079));
#5310=CLOSED_SHELL('',(#5080));
#5311=CLOSED_SHELL('',(#5081));
#5312=CLOSED_SHELL('',(#5082));
#5313=CLOSED_SHELL('',(#5083,#5084,#5085,#5086,#5087,#5088,#5089,#5090,
#5091,#5092,#5093,#5094,#5095,#5096,#5097,#5098,#5099));
#5314=CLOSED_SHELL('',(#5100,#5101,#5102,#5103));
#5315=CLOSED_SHELL('',(#5104,#5105,#5106,#5107));
#5316=CLOSED_SHELL('',(#5108,#5109,#5110,#5111,#5112,#5113,#5114,#5115,
#5116,#5117,#5118,#5119));
#5317=CLOSED_SHELL('',(#5120,#5121,#5122,#5123,#5124,#5125,#5126,#5127,
#5128,#5129,#5130,#5131,#5132,#5133,#5134,#5135,#5136,#5137,#5138,#5139,
#5140,#5141,#5142,#5143));
#5318=CLOSED_SHELL('',(#5144,#5145,#5146,#5147));
#5319=CLOSED_SHELL('',(#5148,#5149,#5150,#5151,#5152,#5153,#5154));
#5320=CLOSED_SHELL('',(#5155,#5156,#5157,#5158,#5159,#5160,#5161,#5162,
#5163,#5164,#5165));
#5321=CLOSED_SHELL('',(#5166,#5167,#5168,#5169));
#5322=CLOSED_SHELL('',(#5170,#5171,#5172,#5173));
#5323=CLOSED_SHELL('',(#5174,#5175,#5176,#5177,#5178,#5179,#5180,#5181,
#5182,#5183,#5184,#5185,#5186,#5187));
#5324=CLOSED_SHELL('',(#5188,#5189,#5190,#5191,#5192,#5193,#5194,#5195,
#5196,#5197,#5198,#5199));
#5325=CLOSED_SHELL('',(#5200,#5201,#5202,#5203,#5204,#5205,#5206,#5207));
#5326=CLOSED_SHELL('',(#5208,#5209,#5210,#5211,#5212,#5213,#5214,#5215));
#5327=CLOSED_SHELL('',(#5216,#5217,#5218,#5219,#5220,#5221,#5222,#5223));
#5328=CLOSED_SHELL('',(#5224,#5225,#5226,#5227,#5228,#5229,#5230,#5231));
#5329=CLOSED_SHELL('',(#5232));
#5330=CLOSED_SHELL('',(#5233));
#5331=CLOSED_SHELL('',(#5234));
#5332=CLOSED_SHELL('',(#5235));
#5333=CLOSED_SHELL('',(#5236));
#5334=CLOSED_SHELL('',(#5237));
#5335=CLOSED_SHELL('',(#5238));
#5336=CLOSED_SHELL('',(#5239));
#5337=CLOSED_SHELL('',(#5240,#5241,#5242,#5243,#5244,#5245,#5246,#5247,
#5248,#5249,#5250,#5251,#5252,#5253,#5254,#5255,#5256,#5257,#5258));
#5338=CLOSED_SHELL('',(#5259,#5260,#5261,#5262));
#5339=CLOSED_SHELL('',(#5263,#5264,#5265,#5266));
#5340=CLOSED_SHELL('',(#5267,#5268,#5269,#5270,#5271,#5272,#5273,#5274,
#5275));
#5341=CLOSED_SHELL('',(#5276,#5277,#5278,#5279,#5280,#5281,#5282,#5283));
#5342=CLOSED_SHELL('',(#5284,#5285,#5286,#5287,#5288,#5289));
#5343=CLOSED_SHELL('',(#5290,#5291,#5292,#5293));
#5344=DERIVED_UNIT_ELEMENT(#5408,1.);
#5345=DERIVED_UNIT_ELEMENT(#10512,-3.);
#5346=DERIVED_UNIT_ELEMENT(#5408,1.);
#5347=DERIVED_UNIT_ELEMENT(#10512,-3.);
#5348=DERIVED_UNIT_ELEMENT(#5408,1.);
#5349=DERIVED_UNIT_ELEMENT(#10512,-3.);
#5350=DERIVED_UNIT_ELEMENT(#5408,1.);
#5351=DERIVED_UNIT_ELEMENT(#10512,-3.);
#5352=DERIVED_UNIT_ELEMENT(#5408,1.);
#5353=DERIVED_UNIT_ELEMENT(#10512,-3.);
#5354=DERIVED_UNIT_ELEMENT(#5408,1.);
#5355=DERIVED_UNIT_ELEMENT(#10512,-3.);
#5356=DERIVED_UNIT_ELEMENT(#5408,1.);
#5357=DERIVED_UNIT_ELEMENT(#10512,-3.);
#5358=DERIVED_UNIT_ELEMENT(#5408,1.);
#5359=DERIVED_UNIT_ELEMENT(#10512,-3.);
#5360=DERIVED_UNIT_ELEMENT(#5408,1.);
#5361=DERIVED_UNIT_ELEMENT(#10512,-3.);
#5362=DERIVED_UNIT_ELEMENT(#5408,1.);
#5363=DERIVED_UNIT_ELEMENT(#10512,-3.);
#5364=DERIVED_UNIT_ELEMENT(#5408,1.);
#5365=DERIVED_UNIT_ELEMENT(#10512,-3.);
#5366=DERIVED_UNIT_ELEMENT(#5408,1.);
#5367=DERIVED_UNIT_ELEMENT(#10512,-3.);
#5368=DERIVED_UNIT_ELEMENT(#5408,1.);
#5369=DERIVED_UNIT_ELEMENT(#10512,-3.);
#5370=DERIVED_UNIT_ELEMENT(#5408,1.);
#5371=DERIVED_UNIT_ELEMENT(#10512,-3.);
#5372=DERIVED_UNIT_ELEMENT(#5408,1.);
#5373=DERIVED_UNIT_ELEMENT(#10512,-3.);
#5374=DERIVED_UNIT_ELEMENT(#5408,1.);
#5375=DERIVED_UNIT_ELEMENT(#10512,-3.);
#5376=DERIVED_UNIT_ELEMENT(#5408,1.);
#5377=DERIVED_UNIT_ELEMENT(#10512,-3.);
#5378=DERIVED_UNIT_ELEMENT(#5408,1.);
#5379=DERIVED_UNIT_ELEMENT(#10512,-3.);
#5380=DERIVED_UNIT_ELEMENT(#5408,1.);
#5381=DERIVED_UNIT_ELEMENT(#10512,-3.);
#5382=DERIVED_UNIT_ELEMENT(#5408,1.);
#5383=DERIVED_UNIT_ELEMENT(#10512,-3.);
#5384=DERIVED_UNIT_ELEMENT(#5408,1.);
#5385=DERIVED_UNIT_ELEMENT(#10512,-3.);
#5386=DERIVED_UNIT_ELEMENT(#5408,1.);
#5387=DERIVED_UNIT_ELEMENT(#10512,-3.);
#5388=DERIVED_UNIT_ELEMENT(#5408,1.);
#5389=DERIVED_UNIT_ELEMENT(#10512,-3.);
#5390=DERIVED_UNIT_ELEMENT(#5408,1.);
#5391=DERIVED_UNIT_ELEMENT(#10512,-3.);
#5392=DERIVED_UNIT_ELEMENT(#5408,1.);
#5393=DERIVED_UNIT_ELEMENT(#10512,-3.);
#5394=DERIVED_UNIT_ELEMENT(#5408,1.);
#5395=DERIVED_UNIT_ELEMENT(#10512,-3.);
#5396=DERIVED_UNIT_ELEMENT(#5408,1.);
#5397=DERIVED_UNIT_ELEMENT(#10512,-3.);
#5398=DERIVED_UNIT_ELEMENT(#5408,1.);
#5399=DERIVED_UNIT_ELEMENT(#10512,-3.);
#5400=DERIVED_UNIT_ELEMENT(#5408,1.);
#5401=DERIVED_UNIT_ELEMENT(#10512,-3.);
#5402=DERIVED_UNIT_ELEMENT(#5408,1.);
#5403=DERIVED_UNIT_ELEMENT(#10512,-3.);
#5404=DERIVED_UNIT_ELEMENT(#5408,1.);
#5405=DERIVED_UNIT_ELEMENT(#10512,-3.);
#5406=DERIVED_UNIT_ELEMENT(#5408,1.);
#5407=DERIVED_UNIT_ELEMENT(#10512,-3.);
#5408=(
MASS_UNIT()
NAMED_UNIT(*)
SI_UNIT(.KILO.,.GRAM.)
);
#5409=DERIVED_UNIT((#5344,#5345));
#5410=DERIVED_UNIT((#5346,#5347));
#5411=DERIVED_UNIT((#5348,#5349));
#5412=DERIVED_UNIT((#5350,#5351));
#5413=DERIVED_UNIT((#5352,#5353));
#5414=DERIVED_UNIT((#5354,#5355));
#5415=DERIVED_UNIT((#5356,#5357));
#5416=DERIVED_UNIT((#5358,#5359));
#5417=DERIVED_UNIT((#5360,#5361));
#5418=DERIVED_UNIT((#5362,#5363));
#5419=DERIVED_UNIT((#5364,#5365));
#5420=DERIVED_UNIT((#5366,#5367));
#5421=DERIVED_UNIT((#5368,#5369));
#5422=DERIVED_UNIT((#5370,#5371));
#5423=DERIVED_UNIT((#5372,#5373));
#5424=DERIVED_UNIT((#5374,#5375));
#5425=DERIVED_UNIT((#5376,#5377));
#5426=DERIVED_UNIT((#5378,#5379));
#5427=DERIVED_UNIT((#5380,#5381));
#5428=DERIVED_UNIT((#5382,#5383));
#5429=DERIVED_UNIT((#5384,#5385));
#5430=DERIVED_UNIT((#5386,#5387));
#5431=DERIVED_UNIT((#5388,#5389));
#5432=DERIVED_UNIT((#5390,#5391));
#5433=DERIVED_UNIT((#5392,#5393));
#5434=DERIVED_UNIT((#5394,#5395));
#5435=DERIVED_UNIT((#5396,#5397));
#5436=DERIVED_UNIT((#5398,#5399));
#5437=DERIVED_UNIT((#5400,#5401));
#5438=DERIVED_UNIT((#5402,#5403));
#5439=DERIVED_UNIT((#5404,#5405));
#5440=DERIVED_UNIT((#5406,#5407));
#5441=MEASURE_REPRESENTATION_ITEM('density measure',
POSITIVE_RATIO_MEASURE(7850.),#5409);
#5442=MEASURE_REPRESENTATION_ITEM('density measure',
POSITIVE_RATIO_MEASURE(7850.),#5410);
#5443=MEASURE_REPRESENTATION_ITEM('density measure',
POSITIVE_RATIO_MEASURE(7850.),#5411);
#5444=MEASURE_REPRESENTATION_ITEM('density measure',
POSITIVE_RATIO_MEASURE(7850.),#5412);
#5445=MEASURE_REPRESENTATION_ITEM('density measure',
POSITIVE_RATIO_MEASURE(7850.),#5413);
#5446=MEASURE_REPRESENTATION_ITEM('density measure',
POSITIVE_RATIO_MEASURE(7850.),#5414);
#5447=MEASURE_REPRESENTATION_ITEM('density measure',
POSITIVE_RATIO_MEASURE(7850.),#5415);
#5448=MEASURE_REPRESENTATION_ITEM('density measure',
POSITIVE_RATIO_MEASURE(7850.),#5416);
#5449=MEASURE_REPRESENTATION_ITEM('density measure',
POSITIVE_RATIO_MEASURE(7850.),#5417);
#5450=MEASURE_REPRESENTATION_ITEM('density measure',
POSITIVE_RATIO_MEASURE(7850.),#5418);
#5451=MEASURE_REPRESENTATION_ITEM('density measure',
POSITIVE_RATIO_MEASURE(7850.),#5419);
#5452=MEASURE_REPRESENTATION_ITEM('density measure',
POSITIVE_RATIO_MEASURE(7850.),#5420);
#5453=MEASURE_REPRESENTATION_ITEM('density measure',
POSITIVE_RATIO_MEASURE(7850.),#5421);
#5454=MEASURE_REPRESENTATION_ITEM('density measure',
POSITIVE_RATIO_MEASURE(7850.),#5422);
#5455=MEASURE_REPRESENTATION_ITEM('density measure',
POSITIVE_RATIO_MEASURE(7850.),#5423);
#5456=MEASURE_REPRESENTATION_ITEM('density measure',
POSITIVE_RATIO_MEASURE(7850.),#5424);
#5457=MEASURE_REPRESENTATION_ITEM('density measure',
POSITIVE_RATIO_MEASURE(7850.),#5425);
#5458=MEASURE_REPRESENTATION_ITEM('density measure',
POSITIVE_RATIO_MEASURE(7850.),#5426);
#5459=MEASURE_REPRESENTATION_ITEM('density measure',
POSITIVE_RATIO_MEASURE(7850.),#5427);
#5460=MEASURE_REPRESENTATION_ITEM('density measure',
POSITIVE_RATIO_MEASURE(7850.),#5428);
#5461=MEASURE_REPRESENTATION_ITEM('density measure',
POSITIVE_RATIO_MEASURE(7850.),#5429);
#5462=MEASURE_REPRESENTATION_ITEM('density measure',
POSITIVE_RATIO_MEASURE(7850.),#5430);
#5463=MEASURE_REPRESENTATION_ITEM('density measure',
POSITIVE_RATIO_MEASURE(7850.),#5431);
#5464=MEASURE_REPRESENTATION_ITEM('density measure',
POSITIVE_RATIO_MEASURE(7850.),#5432);
#5465=MEASURE_REPRESENTATION_ITEM('density measure',
POSITIVE_RATIO_MEASURE(7850.),#5433);
#5466=MEASURE_REPRESENTATION_ITEM('density measure',
POSITIVE_RATIO_MEASURE(7850.),#5434);
#5467=MEASURE_REPRESENTATION_ITEM('density measure',
POSITIVE_RATIO_MEASURE(7850.),#5435);
#5468=MEASURE_REPRESENTATION_ITEM('density measure',
POSITIVE_RATIO_MEASURE(7850.),#5436);
#5469=MEASURE_REPRESENTATION_ITEM('density measure',
POSITIVE_RATIO_MEASURE(7850.),#5437);
#5470=MEASURE_REPRESENTATION_ITEM('density measure',
POSITIVE_RATIO_MEASURE(7850.),#5438);
#5471=MEASURE_REPRESENTATION_ITEM('density measure',
POSITIVE_RATIO_MEASURE(7850.),#5439);
#5472=MEASURE_REPRESENTATION_ITEM('density measure',
POSITIVE_RATIO_MEASURE(7850.),#5440);
#5473=PROPERTY_DEFINITION_REPRESENTATION(#5633,#5537);
#5474=PROPERTY_DEFINITION_REPRESENTATION(#5634,#5538);
#5475=PROPERTY_DEFINITION_REPRESENTATION(#5635,#5539);
#5476=PROPERTY_DEFINITION_REPRESENTATION(#5636,#5540);
#5477=PROPERTY_DEFINITION_REPRESENTATION(#5637,#5541);
#5478=PROPERTY_DEFINITION_REPRESENTATION(#5638,#5542);
#5479=PROPERTY_DEFINITION_REPRESENTATION(#5639,#5543);
#5480=PROPERTY_DEFINITION_REPRESENTATION(#5640,#5544);
#5481=PROPERTY_DEFINITION_REPRESENTATION(#5641,#5545);
#5482=PROPERTY_DEFINITION_REPRESENTATION(#5642,#5546);
#5483=PROPERTY_DEFINITION_REPRESENTATION(#5643,#5547);
#5484=PROPERTY_DEFINITION_REPRESENTATION(#5644,#5548);
#5485=PROPERTY_DEFINITION_REPRESENTATION(#5645,#5549);
#5486=PROPERTY_DEFINITION_REPRESENTATION(#5646,#5550);
#5487=PROPERTY_DEFINITION_REPRESENTATION(#5647,#5551);
#5488=PROPERTY_DEFINITION_REPRESENTATION(#5648,#5552);
#5489=PROPERTY_DEFINITION_REPRESENTATION(#5649,#5553);
#5490=PROPERTY_DEFINITION_REPRESENTATION(#5650,#5554);
#5491=PROPERTY_DEFINITION_REPRESENTATION(#5651,#5555);
#5492=PROPERTY_DEFINITION_REPRESENTATION(#5652,#5556);
#5493=PROPERTY_DEFINITION_REPRESENTATION(#5653,#5557);
#5494=PROPERTY_DEFINITION_REPRESENTATION(#5654,#5558);
#5495=PROPERTY_DEFINITION_REPRESENTATION(#5655,#5559);
#5496=PROPERTY_DEFINITION_REPRESENTATION(#5656,#5560);
#5497=PROPERTY_DEFINITION_REPRESENTATION(#5657,#5561);
#5498=PROPERTY_DEFINITION_REPRESENTATION(#5658,#5562);
#5499=PROPERTY_DEFINITION_REPRESENTATION(#5659,#5563);
#5500=PROPERTY_DEFINITION_REPRESENTATION(#5660,#5564);
#5501=PROPERTY_DEFINITION_REPRESENTATION(#5661,#5565);
#5502=PROPERTY_DEFINITION_REPRESENTATION(#5662,#5566);
#5503=PROPERTY_DEFINITION_REPRESENTATION(#5663,#5567);
#5504=PROPERTY_DEFINITION_REPRESENTATION(#5664,#5568);
#5505=PROPERTY_DEFINITION_REPRESENTATION(#5665,#5569);
#5506=PROPERTY_DEFINITION_REPRESENTATION(#5666,#5570);
#5507=PROPERTY_DEFINITION_REPRESENTATION(#5667,#5571);
#5508=PROPERTY_DEFINITION_REPRESENTATION(#5668,#5572);
#5509=PROPERTY_DEFINITION_REPRESENTATION(#5669,#5573);
#5510=PROPERTY_DEFINITION_REPRESENTATION(#5670,#5574);
#5511=PROPERTY_DEFINITION_REPRESENTATION(#5671,#5575);
#5512=PROPERTY_DEFINITION_REPRESENTATION(#5672,#5576);
#5513=PROPERTY_DEFINITION_REPRESENTATION(#5673,#5577);
#5514=PROPERTY_DEFINITION_REPRESENTATION(#5674,#5578);
#5515=PROPERTY_DEFINITION_REPRESENTATION(#5675,#5579);
#5516=PROPERTY_DEFINITION_REPRESENTATION(#5676,#5580);
#5517=PROPERTY_DEFINITION_REPRESENTATION(#5677,#5581);
#5518=PROPERTY_DEFINITION_REPRESENTATION(#5678,#5582);
#5519=PROPERTY_DEFINITION_REPRESENTATION(#5679,#5583);
#5520=PROPERTY_DEFINITION_REPRESENTATION(#5680,#5584);
#5521=PROPERTY_DEFINITION_REPRESENTATION(#5681,#5585);
#5522=PROPERTY_DEFINITION_REPRESENTATION(#5682,#5586);
#5523=PROPERTY_DEFINITION_REPRESENTATION(#5683,#5587);
#5524=PROPERTY_DEFINITION_REPRESENTATION(#5684,#5588);
#5525=PROPERTY_DEFINITION_REPRESENTATION(#5685,#5589);
#5526=PROPERTY_DEFINITION_REPRESENTATION(#5686,#5590);
#5527=PROPERTY_DEFINITION_REPRESENTATION(#5687,#5591);
#5528=PROPERTY_DEFINITION_REPRESENTATION(#5688,#5592);
#5529=PROPERTY_DEFINITION_REPRESENTATION(#5689,#5593);
#5530=PROPERTY_DEFINITION_REPRESENTATION(#5690,#5594);
#5531=PROPERTY_DEFINITION_REPRESENTATION(#5691,#5595);
#5532=PROPERTY_DEFINITION_REPRESENTATION(#5692,#5596);
#5533=PROPERTY_DEFINITION_REPRESENTATION(#5693,#5597);
#5534=PROPERTY_DEFINITION_REPRESENTATION(#5694,#5598);
#5535=PROPERTY_DEFINITION_REPRESENTATION(#5695,#5599);
#5536=PROPERTY_DEFINITION_REPRESENTATION(#5696,#5600);
#5537=REPRESENTATION('material name',(#5601),#10474);
#5538=REPRESENTATION('density',(#5441),#10474);
#5539=REPRESENTATION('material name',(#5602),#10475);
#5540=REPRESENTATION('density',(#5442),#10475);
#5541=REPRESENTATION('material name',(#5603),#10476);
#5542=REPRESENTATION('density',(#5443),#10476);
#5543=REPRESENTATION('material name',(#5604),#10477);
#5544=REPRESENTATION('density',(#5444),#10477);
#5545=REPRESENTATION('material name',(#5605),#10478);
#5546=REPRESENTATION('density',(#5445),#10478);
#5547=REPRESENTATION('material name',(#5606),#10479);
#5548=REPRESENTATION('density',(#5446),#10479);
#5549=REPRESENTATION('material name',(#5607),#10480);
#5550=REPRESENTATION('density',(#5447),#10480);
#5551=REPRESENTATION('material name',(#5608),#10481);
#5552=REPRESENTATION('density',(#5448),#10481);
#5553=REPRESENTATION('material name',(#5609),#10482);
#5554=REPRESENTATION('density',(#5449),#10482);
#5555=REPRESENTATION('material name',(#5610),#10484);
#5556=REPRESENTATION('density',(#5450),#10484);
#5557=REPRESENTATION('material name',(#5611),#10485);
#5558=REPRESENTATION('density',(#5451),#10485);
#5559=REPRESENTATION('material name',(#5612),#10486);
#5560=REPRESENTATION('density',(#5452),#10486);
#5561=REPRESENTATION('material name',(#5613),#10487);
#5562=REPRESENTATION('density',(#5453),#10487);
#5563=REPRESENTATION('material name',(#5614),#10488);
#5564=REPRESENTATION('density',(#5454),#10488);
#5565=REPRESENTATION('material name',(#5615),#10490);
#5566=REPRESENTATION('density',(#5455),#10490);
#5567=REPRESENTATION('material name',(#5616),#10491);
#5568=REPRESENTATION('density',(#5456),#10491);
#5569=REPRESENTATION('material name',(#5617),#10492);
#5570=REPRESENTATION('density',(#5457),#10492);
#5571=REPRESENTATION('material name',(#5618),#10493);
#5572=REPRESENTATION('density',(#5458),#10493);
#5573=REPRESENTATION('material name',(#5619),#10494);
#5574=REPRESENTATION('density',(#5459),#10494);
#5575=REPRESENTATION('material name',(#5620),#10495);
#5576=REPRESENTATION('density',(#5460),#10495);
#5577=REPRESENTATION('material name',(#5621),#10496);
#5578=REPRESENTATION('density',(#5461),#10496);
#5579=REPRESENTATION('material name',(#5622),#10497);
#5580=REPRESENTATION('density',(#5462),#10497);
#5581=REPRESENTATION('material name',(#5623),#10498);
#5582=REPRESENTATION('density',(#5463),#10498);
#5583=REPRESENTATION('material name',(#5624),#10499);
#5584=REPRESENTATION('density',(#5464),#10499);
#5585=REPRESENTATION('material name',(#5625),#10501);
#5586=REPRESENTATION('density',(#5465),#10501);
#5587=REPRESENTATION('material name',(#5626),#10502);
#5588=REPRESENTATION('density',(#5466),#10502);
#5589=REPRESENTATION('material name',(#5627),#10503);
#5590=REPRESENTATION('density',(#5467),#10503);
#5591=REPRESENTATION('material name',(#5628),#10504);
#5592=REPRESENTATION('density',(#5468),#10504);
#5593=REPRESENTATION('material name',(#5629),#10505);
#5594=REPRESENTATION('density',(#5469),#10505);
#5595=REPRESENTATION('material name',(#5630),#10506);
#5596=REPRESENTATION('density',(#5470),#10506);
#5597=REPRESENTATION('material name',(#5631),#10508);
#5598=REPRESENTATION('density',(#5471),#10508);
#5599=REPRESENTATION('material name',(#5632),#10509);
#5600=REPRESENTATION('density',(#5472),#10509);
#5601=DESCRIPTIVE_REPRESENTATION_ITEM('Steel','Steel');
#5602=DESCRIPTIVE_REPRESENTATION_ITEM('Steel','Steel');
#5603=DESCRIPTIVE_REPRESENTATION_ITEM('Steel','Steel');
#5604=DESCRIPTIVE_REPRESENTATION_ITEM('Steel','Steel');
#5605=DESCRIPTIVE_REPRESENTATION_ITEM('Steel','Steel');
#5606=DESCRIPTIVE_REPRESENTATION_ITEM('Steel','Steel');
#5607=DESCRIPTIVE_REPRESENTATION_ITEM('Steel','Steel');
#5608=DESCRIPTIVE_REPRESENTATION_ITEM('Steel','Steel');
#5609=DESCRIPTIVE_REPRESENTATION_ITEM('Steel','Steel');
#5610=DESCRIPTIVE_REPRESENTATION_ITEM('Steel','Steel');
#5611=DESCRIPTIVE_REPRESENTATION_ITEM('Steel','Steel');
#5612=DESCRIPTIVE_REPRESENTATION_ITEM('Steel','Steel');
#5613=DESCRIPTIVE_REPRESENTATION_ITEM('Steel','Steel');
#5614=DESCRIPTIVE_REPRESENTATION_ITEM('Steel','Steel');
#5615=DESCRIPTIVE_REPRESENTATION_ITEM('Steel','Steel');
#5616=DESCRIPTIVE_REPRESENTATION_ITEM('Steel','Steel');
#5617=DESCRIPTIVE_REPRESENTATION_ITEM('Steel','Steel');
#5618=DESCRIPTIVE_REPRESENTATION_ITEM('Steel','Steel');
#5619=DESCRIPTIVE_REPRESENTATION_ITEM('Steel','Steel');
#5620=DESCRIPTIVE_REPRESENTATION_ITEM('Steel','Steel');
#5621=DESCRIPTIVE_REPRESENTATION_ITEM('Steel','Steel');
#5622=DESCRIPTIVE_REPRESENTATION_ITEM('Steel','Steel');
#5623=DESCRIPTIVE_REPRESENTATION_ITEM('Steel','Steel');
#5624=DESCRIPTIVE_REPRESENTATION_ITEM('Steel','Steel');
#5625=DESCRIPTIVE_REPRESENTATION_ITEM('Steel','Steel');
#5626=DESCRIPTIVE_REPRESENTATION_ITEM('Steel','Steel');
#5627=DESCRIPTIVE_REPRESENTATION_ITEM('Steel','Steel');
#5628=DESCRIPTIVE_REPRESENTATION_ITEM('Steel','Steel');
#5629=DESCRIPTIVE_REPRESENTATION_ITEM('Steel','Steel');
#5630=DESCRIPTIVE_REPRESENTATION_ITEM('Steel','Steel');
#5631=DESCRIPTIVE_REPRESENTATION_ITEM('Steel','Steel');
#5632=DESCRIPTIVE_REPRESENTATION_ITEM('Steel','Steel');
#5633=PROPERTY_DEFINITION('material property','material name',#10686);
#5634=PROPERTY_DEFINITION('material property','density of part',#10686);
#5635=PROPERTY_DEFINITION('material property','material name',#10687);
#5636=PROPERTY_DEFINITION('material property','density of part',#10687);
#5637=PROPERTY_DEFINITION('material property','material name',#10688);
#5638=PROPERTY_DEFINITION('material property','density of part',#10688);
#5639=PROPERTY_DEFINITION('material property','material name',#10689);
#5640=PROPERTY_DEFINITION('material property','density of part',#10689);
#5641=PROPERTY_DEFINITION('material property','material name',#10690);
#5642=PROPERTY_DEFINITION('material property','density of part',#10690);
#5643=PROPERTY_DEFINITION('material property','material name',#10691);
#5644=PROPERTY_DEFINITION('material property','density of part',#10691);
#5645=PROPERTY_DEFINITION('material property','material name',#10692);
#5646=PROPERTY_DEFINITION('material property','density of part',#10692);
#5647=PROPERTY_DEFINITION('material property','material name',#10693);
#5648=PROPERTY_DEFINITION('material property','density of part',#10693);
#5649=PROPERTY_DEFINITION('material property','material name',#10694);
#5650=PROPERTY_DEFINITION('material property','density of part',#10694);
#5651=PROPERTY_DEFINITION('material property','material name',#10696);
#5652=PROPERTY_DEFINITION('material property','density of part',#10696);
#5653=PROPERTY_DEFINITION('material property','material name',#10697);
#5654=PROPERTY_DEFINITION('material property','density of part',#10697);
#5655=PROPERTY_DEFINITION('material property','material name',#10698);
#5656=PROPERTY_DEFINITION('material property','density of part',#10698);
#5657=PROPERTY_DEFINITION('material property','material name',#10699);
#5658=PROPERTY_DEFINITION('material property','density of part',#10699);
#5659=PROPERTY_DEFINITION('material property','material name',#10700);
#5660=PROPERTY_DEFINITION('material property','density of part',#10700);
#5661=PROPERTY_DEFINITION('material property','material name',#10702);
#5662=PROPERTY_DEFINITION('material property','density of part',#10702);
#5663=PROPERTY_DEFINITION('material property','material name',#10703);
#5664=PROPERTY_DEFINITION('material property','density of part',#10703);
#5665=PROPERTY_DEFINITION('material property','material name',#10704);
#5666=PROPERTY_DEFINITION('material property','density of part',#10704);
#5667=PROPERTY_DEFINITION('material property','material name',#10705);
#5668=PROPERTY_DEFINITION('material property','density of part',#10705);
#5669=PROPERTY_DEFINITION('material property','material name',#10706);
#5670=PROPERTY_DEFINITION('material property','density of part',#10706);
#5671=PROPERTY_DEFINITION('material property','material name',#10707);
#5672=PROPERTY_DEFINITION('material property','density of part',#10707);
#5673=PROPERTY_DEFINITION('material property','material name',#10708);
#5674=PROPERTY_DEFINITION('material property','density of part',#10708);
#5675=PROPERTY_DEFINITION('material property','material name',#10709);
#5676=PROPERTY_DEFINITION('material property','density of part',#10709);
#5677=PROPERTY_DEFINITION('material property','material name',#10710);
#5678=PROPERTY_DEFINITION('material property','density of part',#10710);
#5679=PROPERTY_DEFINITION('material property','material name',#10711);
#5680=PROPERTY_DEFINITION('material property','density of part',#10711);
#5681=PROPERTY_DEFINITION('material property','material name',#10713);
#5682=PROPERTY_DEFINITION('material property','density of part',#10713);
#5683=PROPERTY_DEFINITION('material property','material name',#10714);
#5684=PROPERTY_DEFINITION('material property','density of part',#10714);
#5685=PROPERTY_DEFINITION('material property','material name',#10715);
#5686=PROPERTY_DEFINITION('material property','density of part',#10715);
#5687=PROPERTY_DEFINITION('material property','material name',#10716);
#5688=PROPERTY_DEFINITION('material property','density of part',#10716);
#5689=PROPERTY_DEFINITION('material property','material name',#10717);
#5690=PROPERTY_DEFINITION('material property','density of part',#10717);
#5691=PROPERTY_DEFINITION('material property','material name',#10718);
#5692=PROPERTY_DEFINITION('material property','density of part',#10718);
#5693=PROPERTY_DEFINITION('material property','material name',#10720);
#5694=PROPERTY_DEFINITION('material property','density of part',#10720);
#5695=PROPERTY_DEFINITION('material property','material name',#10721);
#5696=PROPERTY_DEFINITION('material property','density of part',#10721);
#5697=AXIS2_PLACEMENT_3D('',#8173,#6419,#6420);
#5698=AXIS2_PLACEMENT_3D('',#8174,#6421,#6422);
#5699=AXIS2_PLACEMENT_3D('',#8175,#6423,#6424);
#5700=AXIS2_PLACEMENT_3D('',#8176,#6425,#6426);
#5701=AXIS2_PLACEMENT_3D('',#8178,#6427,#6428);
#5702=AXIS2_PLACEMENT_3D('',#8181,#6430,#6431);
#5703=AXIS2_PLACEMENT_3D('',#8182,#6432,#6433);
#5704=AXIS2_PLACEMENT_3D('',#8184,#6434,#6435);
#5705=AXIS2_PLACEMENT_3D('',#8187,#6437,#6438);
#5706=AXIS2_PLACEMENT_3D('',#8188,#6439,#6440);
#5707=AXIS2_PLACEMENT_3D('',#8190,#6441,#6442);
#5708=AXIS2_PLACEMENT_3D('',#8193,#6444,#6445);
#5709=AXIS2_PLACEMENT_3D('',#8194,#6446,#6447);
#5710=AXIS2_PLACEMENT_3D('',#8196,#6448,#6449);
#5711=AXIS2_PLACEMENT_3D('',#8199,#6451,#6452);
#5712=AXIS2_PLACEMENT_3D('',#8200,#6453,#6454);
#5713=AXIS2_PLACEMENT_3D('',#8209,#6459,#6460);
#5714=AXIS2_PLACEMENT_3D('',#8215,#6464,#6465);
#5715=AXIS2_PLACEMENT_3D('',#8221,#6469,#6470);
#5716=AXIS2_PLACEMENT_3D('',#8224,#6473,#6474);
#5717=AXIS2_PLACEMENT_3D('',#8225,#6475,#6476);
#5718=AXIS2_PLACEMENT_3D('',#8226,#6477,#6478);
#5719=AXIS2_PLACEMENT_3D('',#8227,#6479,#6480);
#5720=AXIS2_PLACEMENT_3D('',#8236,#6485,#6486);
#5721=AXIS2_PLACEMENT_3D('',#8242,#6490,#6491);
#5722=AXIS2_PLACEMENT_3D('',#8248,#6495,#6496);
#5723=AXIS2_PLACEMENT_3D('',#8251,#6499,#6500);
#5724=AXIS2_PLACEMENT_3D('',#8252,#6501,#6502);
#5725=AXIS2_PLACEMENT_3D('',#8253,#6503,#6504);
#5726=AXIS2_PLACEMENT_3D('',#8254,#6505,#6506);
#5727=AXIS2_PLACEMENT_3D('',#8263,#6511,#6512);
#5728=AXIS2_PLACEMENT_3D('',#8269,#6516,#6517);
#5729=AXIS2_PLACEMENT_3D('',#8275,#6521,#6522);
#5730=AXIS2_PLACEMENT_3D('',#8278,#6525,#6526);
#5731=AXIS2_PLACEMENT_3D('',#8279,#6527,#6528);
#5732=AXIS2_PLACEMENT_3D('',#8280,#6529,#6530);
#5733=AXIS2_PLACEMENT_3D('',#8281,#6531,#6532);
#5734=AXIS2_PLACEMENT_3D('',#8283,#6533,#6534);
#5735=AXIS2_PLACEMENT_3D('',#8286,#6536,#6537);
#5736=AXIS2_PLACEMENT_3D('',#8287,#6538,#6539);
#5737=AXIS2_PLACEMENT_3D('',#8289,#6540,#6541);
#5738=AXIS2_PLACEMENT_3D('',#8292,#6543,#6544);
#5739=AXIS2_PLACEMENT_3D('',#8293,#6545,#6546);
#5740=AXIS2_PLACEMENT_3D('',#8295,#6547,#6548);
#5741=AXIS2_PLACEMENT_3D('',#8298,#6550,#6551);
#5742=AXIS2_PLACEMENT_3D('',#8299,#6552,#6553);
#5743=AXIS2_PLACEMENT_3D('',#8301,#6554,#6555);
#5744=AXIS2_PLACEMENT_3D('',#8304,#6557,#6558);
#5745=AXIS2_PLACEMENT_3D('',#8305,#6559,#6560);
#5746=AXIS2_PLACEMENT_3D('',#8307,#6561,#6562);
#5747=AXIS2_PLACEMENT_3D('',#8310,#6564,#6565);
#5748=AXIS2_PLACEMENT_3D('',#8311,#6566,#6567);
#5749=AXIS2_PLACEMENT_3D('',#8313,#6568,#6569);
#5750=AXIS2_PLACEMENT_3D('',#8316,#6571,#6572);
#5751=AXIS2_PLACEMENT_3D('',#8317,#6573,#6574);
#5752=AXIS2_PLACEMENT_3D('',#8319,#6575,#6576);
#5753=AXIS2_PLACEMENT_3D('',#8322,#6578,#6579);
#5754=AXIS2_PLACEMENT_3D('',#8323,#6580,#6581);
#5755=AXIS2_PLACEMENT_3D('',#8325,#6582,#6583);
#5756=AXIS2_PLACEMENT_3D('',#8328,#6585,#6586);
#5757=AXIS2_PLACEMENT_3D('',#8329,#6587,#6588);
#5758=AXIS2_PLACEMENT_3D('',#8331,#6589,#6590);
#5759=AXIS2_PLACEMENT_3D('',#8334,#6592,#6593);
#5760=AXIS2_PLACEMENT_3D('',#8335,#6594,#6595);
#5761=AXIS2_PLACEMENT_3D('',#8344,#6600,#6601);
#5762=AXIS2_PLACEMENT_3D('',#8353,#6606,#6607);
#5763=AXIS2_PLACEMENT_3D('',#8359,#6611,#6612);
#5764=AXIS2_PLACEMENT_3D('',#8365,#6616,#6617);
#5765=AXIS2_PLACEMENT_3D('',#8372,#6622,#6623);
#5766=AXIS2_PLACEMENT_3D('',#8376,#6626,#6627);
#5767=AXIS2_PLACEMENT_3D('',#8381,#6631,#6632);
#5768=AXIS2_PLACEMENT_3D('',#8383,#6634,#6635);
#5769=AXIS2_PLACEMENT_3D('',#8384,#6636,#6637);
#5770=AXIS2_PLACEMENT_3D('',#8385,#6638,#6639);
#5771=AXIS2_PLACEMENT_3D('',#8386,#6640,#6641);
#5772=AXIS2_PLACEMENT_3D('',#8388,#6642,#6643);
#5773=AXIS2_PLACEMENT_3D('',#8391,#6645,#6646);
#5774=AXIS2_PLACEMENT_3D('',#8392,#6647,#6648);
#5775=AXIS2_PLACEMENT_3D('',#8394,#6649,#6650);
#5776=AXIS2_PLACEMENT_3D('',#8397,#6652,#6653);
#5777=AXIS2_PLACEMENT_3D('',#8398,#6654,#6655);
#5778=AXIS2_PLACEMENT_3D('',#8399,#6656,#6657);
#5779=AXIS2_PLACEMENT_3D('',#8400,#6658,#6659);
#5780=AXIS2_PLACEMENT_3D('',#8401,#6660,#6661);
#5781=AXIS2_PLACEMENT_3D('',#8403,#6662,#6663);
#5782=AXIS2_PLACEMENT_3D('',#8406,#6665,#6666);
#5783=AXIS2_PLACEMENT_3D('',#8407,#6667,#6668);
#5784=AXIS2_PLACEMENT_3D('',#8409,#6669,#6670);
#5785=AXIS2_PLACEMENT_3D('',#8412,#6672,#6673);
#5786=AXIS2_PLACEMENT_3D('',#8413,#6674,#6675);
#5787=AXIS2_PLACEMENT_3D('',#8415,#6676,#6677);
#5788=AXIS2_PLACEMENT_3D('',#8418,#6679,#6680);
#5789=AXIS2_PLACEMENT_3D('',#8419,#6681,#6682);
#5790=AXIS2_PLACEMENT_3D('',#8421,#6683,#6684);
#5791=AXIS2_PLACEMENT_3D('',#8424,#6686,#6687);
#5792=AXIS2_PLACEMENT_3D('',#8425,#6688,#6689);
#5793=AXIS2_PLACEMENT_3D('',#8427,#6690,#6691);
#5794=AXIS2_PLACEMENT_3D('',#8430,#6693,#6694);
#5795=AXIS2_PLACEMENT_3D('',#8431,#6695,#6696);
#5796=AXIS2_PLACEMENT_3D('',#8433,#6697,#6698);
#5797=AXIS2_PLACEMENT_3D('',#8434,#6699,#6700);
#5798=AXIS2_PLACEMENT_3D('',#8437,#6702,#6703);
#5799=AXIS2_PLACEMENT_3D('',#8438,#6704,#6705);
#5800=AXIS2_PLACEMENT_3D('',#8440,#6706,#6707);
#5801=AXIS2_PLACEMENT_3D('',#8443,#6709,#6710);
#5802=AXIS2_PLACEMENT_3D('',#8444,#6711,#6712);
#5803=AXIS2_PLACEMENT_3D('',#8445,#6713,#6714);
#5804=AXIS2_PLACEMENT_3D('',#8446,#6715,#6716);
#5805=AXIS2_PLACEMENT_3D('',#8447,#6717,#6718);
#5806=AXIS2_PLACEMENT_3D('',#8449,#6719,#6720);
#5807=AXIS2_PLACEMENT_3D('',#8452,#6722,#6723);
#5808=AXIS2_PLACEMENT_3D('',#8453,#6724,#6725);
#5809=AXIS2_PLACEMENT_3D('',#8455,#6726,#6727);
#5810=AXIS2_PLACEMENT_3D('',#8458,#6729,#6730);
#5811=AXIS2_PLACEMENT_3D('',#8459,#6731,#6732);
#5812=AXIS2_PLACEMENT_3D('',#8461,#6733,#6734);
#5813=AXIS2_PLACEMENT_3D('',#8464,#6736,#6737);
#5814=AXIS2_PLACEMENT_3D('',#8465,#6738,#6739);
#5815=AXIS2_PLACEMENT_3D('',#8467,#6740,#6741);
#5816=AXIS2_PLACEMENT_3D('',#8470,#6743,#6744);
#5817=AXIS2_PLACEMENT_3D('',#8471,#6745,#6746);
#5818=AXIS2_PLACEMENT_3D('',#8473,#6747,#6748);
#5819=AXIS2_PLACEMENT_3D('',#8476,#6750,#6751);
#5820=AXIS2_PLACEMENT_3D('',#8477,#6752,#6753);
#5821=AXIS2_PLACEMENT_3D('',#8479,#6754,#6755);
#5822=AXIS2_PLACEMENT_3D('',#8480,#6756,#6757);
#5823=AXIS2_PLACEMENT_3D('',#8482,#6758,#6759);
#5824=AXIS2_PLACEMENT_3D('',#8484,#6761,#6762);
#5825=AXIS2_PLACEMENT_3D('',#8486,#6763,#6764);
#5826=AXIS2_PLACEMENT_3D('',#8489,#6766,#6767);
#5827=AXIS2_PLACEMENT_3D('',#8490,#6768,#6769);
#5828=AXIS2_PLACEMENT_3D('',#8491,#6770,#6771);
#5829=AXIS2_PLACEMENT_3D('',#8492,#6772,#6773);
#5830=AXIS2_PLACEMENT_3D('',#8493,#6774,#6775);
#5831=AXIS2_PLACEMENT_3D('',#8495,#6776,#6777);
#5832=AXIS2_PLACEMENT_3D('',#8498,#6779,#6780);
#5833=AXIS2_PLACEMENT_3D('',#8499,#6781,#6782);
#5834=AXIS2_PLACEMENT_3D('',#8501,#6783,#6784);
#5835=AXIS2_PLACEMENT_3D('',#8504,#6786,#6787);
#5836=AXIS2_PLACEMENT_3D('',#8505,#6788,#6789);
#5837=AXIS2_PLACEMENT_3D('',#8506,#6790,#6791);
#5838=AXIS2_PLACEMENT_3D('',#8507,#6792,#6793);
#5839=AXIS2_PLACEMENT_3D('',#8508,#6794,#6795);
#5840=AXIS2_PLACEMENT_3D('',#8517,#6800,#6801);
#5841=AXIS2_PLACEMENT_3D('',#8523,#6805,#6806);
#5842=AXIS2_PLACEMENT_3D('',#8529,#6810,#6811);
#5843=AXIS2_PLACEMENT_3D('',#8535,#6815,#6816);
#5844=AXIS2_PLACEMENT_3D('',#8541,#6820,#6821);
#5845=AXIS2_PLACEMENT_3D('',#8544,#6824,#6825);
#5846=AXIS2_PLACEMENT_3D('',#8545,#6826,#6827);
#5847=AXIS2_PLACEMENT_3D('',#8546,#6828,#6829);
#5848=AXIS2_PLACEMENT_3D('',#8548,#6830,#6831);
#5849=AXIS2_PLACEMENT_3D('',#8549,#6832,#6833);
#5850=AXIS2_PLACEMENT_3D('',#8551,#6834,#6835);
#5851=AXIS2_PLACEMENT_3D('',#8552,#6836,#6837);
#5852=AXIS2_PLACEMENT_3D('',#8554,#6838,#6839);
#5853=AXIS2_PLACEMENT_3D('',#8556,#6841,#6842);
#5854=AXIS2_PLACEMENT_3D('',#8558,#6843,#6844);
#5855=AXIS2_PLACEMENT_3D('',#8560,#6846,#6847);
#5856=AXIS2_PLACEMENT_3D('',#8562,#6848,#6849);
#5857=AXIS2_PLACEMENT_3D('',#8564,#6851,#6852);
#5858=AXIS2_PLACEMENT_3D('',#8566,#6853,#6854);
#5859=AXIS2_PLACEMENT_3D('',#8567,#6855,#6856);
#5860=AXIS2_PLACEMENT_3D('',#8569,#6857,#6858);
#5861=AXIS2_PLACEMENT_3D('',#8571,#6860,#6861);
#5862=AXIS2_PLACEMENT_3D('',#8573,#6863,#6864);
#5863=AXIS2_PLACEMENT_3D('',#8574,#6865,#6866);
#5864=AXIS2_PLACEMENT_3D('',#8575,#6867,#6868);
#5865=AXIS2_PLACEMENT_3D('',#8578,#6869,#6870);
#5866=AXIS2_PLACEMENT_3D('',#8579,#6871,#6872);
#5867=AXIS2_PLACEMENT_3D('',#8581,#6873,#6874);
#5868=AXIS2_PLACEMENT_3D('',#8583,#6875,#6876);
#5869=AXIS2_PLACEMENT_3D('',#8584,#6877,#6878);
#5870=AXIS2_PLACEMENT_3D('',#8585,#6879,#6880);
#5871=AXIS2_PLACEMENT_3D('',#8588,#6882,#6883);
#5872=AXIS2_PLACEMENT_3D('',#8589,#6884,#6885);
#5873=AXIS2_PLACEMENT_3D('',#8591,#6886,#6887);
#5874=AXIS2_PLACEMENT_3D('',#8594,#6889,#6890);
#5875=AXIS2_PLACEMENT_3D('',#8595,#6891,#6892);
#5876=AXIS2_PLACEMENT_3D('',#8598,#6894,#6895);
#5877=AXIS2_PLACEMENT_3D('',#8599,#6896,#6897);
#5878=AXIS2_PLACEMENT_3D('',#8600,#6898,#6899);
#5879=AXIS2_PLACEMENT_3D('',#8602,#6900,#6901);
#5880=AXIS2_PLACEMENT_3D('',#8604,#6903,#6904);
#5881=AXIS2_PLACEMENT_3D('',#8606,#6905,#6906);
#5882=AXIS2_PLACEMENT_3D('',#8607,#6907,#6908);
#5883=AXIS2_PLACEMENT_3D('',#8609,#6910,#6911);
#5884=AXIS2_PLACEMENT_3D('',#8610,#6912,#6913);
#5885=AXIS2_PLACEMENT_3D('',#8613,#6914,#6915);
#5886=AXIS2_PLACEMENT_3D('',#8614,#6916,#6917);
#5887=AXIS2_PLACEMENT_3D('',#8616,#6918,#6919);
#5888=AXIS2_PLACEMENT_3D('',#8618,#6920,#6921);
#5889=AXIS2_PLACEMENT_3D('',#8619,#6922,#6923);
#5890=AXIS2_PLACEMENT_3D('',#8620,#6924,#6925);
#5891=AXIS2_PLACEMENT_3D('',#8622,#6926,#6927);
#5892=AXIS2_PLACEMENT_3D('',#8624,#6929,#6930);
#5893=AXIS2_PLACEMENT_3D('',#8626,#6931,#6932);
#5894=AXIS2_PLACEMENT_3D('',#8628,#6933,#6934);
#5895=AXIS2_PLACEMENT_3D('',#8629,#6935,#6936);
#5896=AXIS2_PLACEMENT_3D('',#8631,#6937,#6938);
#5897=AXIS2_PLACEMENT_3D('',#8633,#6940,#6941);
#5898=AXIS2_PLACEMENT_3D('',#8635,#6942,#6943);
#5899=AXIS2_PLACEMENT_3D('',#8637,#6945,#6946);
#5900=AXIS2_PLACEMENT_3D('',#8639,#6947,#6948);
#5901=AXIS2_PLACEMENT_3D('',#8641,#6950,#6951);
#5902=AXIS2_PLACEMENT_3D('',#8642,#6952,#6953);
#5903=AXIS2_PLACEMENT_3D('',#8644,#6955,#6956);
#5904=AXIS2_PLACEMENT_3D('',#8645,#6957,#6958);
#5905=AXIS2_PLACEMENT_3D('',#8648,#6959,#6960);
#5906=AXIS2_PLACEMENT_3D('',#8649,#6961,#6962);
#5907=AXIS2_PLACEMENT_3D('',#8652,#6963,#6964);
#5908=AXIS2_PLACEMENT_3D('',#8653,#6965,#6966);
#5909=AXIS2_PLACEMENT_3D('',#8656,#6967,#6968);
#5910=AXIS2_PLACEMENT_3D('',#8657,#6969,#6970);
#5911=AXIS2_PLACEMENT_3D('',#8660,#6971,#6972);
#5912=AXIS2_PLACEMENT_3D('',#8661,#6973,#6974);
#5913=AXIS2_PLACEMENT_3D('',#8664,#6975,#6976);
#5914=AXIS2_PLACEMENT_3D('',#8665,#6977,#6978);
#5915=AXIS2_PLACEMENT_3D('',#8668,#6979,#6980);
#5916=AXIS2_PLACEMENT_3D('',#8669,#6981,#6982);
#5917=AXIS2_PLACEMENT_3D('',#8672,#6983,#6984);
#5918=AXIS2_PLACEMENT_3D('',#8673,#6985,#6986);
#5919=AXIS2_PLACEMENT_3D('',#8674,#6987,#6988);
#5920=AXIS2_PLACEMENT_3D('',#8700,#6989,#6990);
#5921=AXIS2_PLACEMENT_3D('',#8724,#6991,#6992);
#5922=AXIS2_PLACEMENT_3D('',#8725,#6993,#6994);
#5923=AXIS2_PLACEMENT_3D('',#8727,#6995,#6996);
#5924=AXIS2_PLACEMENT_3D('',#8752,#6997,#6998);
#5925=AXIS2_PLACEMENT_3D('',#8777,#6999,#7000);
#5926=AXIS2_PLACEMENT_3D('',#8780,#7002,#7003);
#5927=AXIS2_PLACEMENT_3D('',#8782,#7004,#7005);
#5928=AXIS2_PLACEMENT_3D('',#8807,#7006,#7007);
#5929=AXIS2_PLACEMENT_3D('',#8832,#7008,#7009);
#5930=AXIS2_PLACEMENT_3D('',#8857,#7010,#7011);
#5931=AXIS2_PLACEMENT_3D('',#8881,#7012,#7013);
#5932=AXIS2_PLACEMENT_3D('',#8882,#7014,#7015);
#5933=AXIS2_PLACEMENT_3D('',#8884,#7016,#7017);
#5934=AXIS2_PLACEMENT_3D('',#8885,#7018,#7019);
#5935=AXIS2_PLACEMENT_3D('',#8886,#7020,#7021);
#5936=AXIS2_PLACEMENT_3D('',#8910,#7022,#7023);
#5937=AXIS2_PLACEMENT_3D('',#8911,#7024,#7025);
#5938=AXIS2_PLACEMENT_3D('',#8913,#7026,#7027);
#5939=AXIS2_PLACEMENT_3D('',#8914,#7028,#7029);
#5940=AXIS2_PLACEMENT_3D('',#8915,#7030,#7031);
#5941=AXIS2_PLACEMENT_3D('',#8939,#7032,#7033);
#5942=AXIS2_PLACEMENT_3D('',#8940,#7034,#7035);
#5943=AXIS2_PLACEMENT_3D('',#8942,#7036,#7037);
#5944=AXIS2_PLACEMENT_3D('',#8944,#7038,#7039);
#5945=AXIS2_PLACEMENT_3D('',#8945,#7040,#7041);
#5946=AXIS2_PLACEMENT_3D('',#8946,#7042,#7043);
#5947=AXIS2_PLACEMENT_3D('',#8970,#7044,#7045);
#5948=AXIS2_PLACEMENT_3D('',#8971,#7046,#7047);
#5949=AXIS2_PLACEMENT_3D('',#8973,#7048,#7049);
#5950=AXIS2_PLACEMENT_3D('',#8974,#7050,#7051);
#5951=AXIS2_PLACEMENT_3D('',#8975,#7052,#7053);
#5952=AXIS2_PLACEMENT_3D('',#8999,#7054,#7055);
#5953=AXIS2_PLACEMENT_3D('',#9000,#7056,#7057);
#5954=AXIS2_PLACEMENT_3D('',#9002,#7058,#7059);
#5955=AXIS2_PLACEMENT_3D('',#9003,#7060,#7061);
#5956=AXIS2_PLACEMENT_3D('',#9004,#7062,#7063);
#5957=AXIS2_PLACEMENT_3D('',#9028,#7064,#7065);
#5958=AXIS2_PLACEMENT_3D('',#9029,#7066,#7067);
#5959=AXIS2_PLACEMENT_3D('',#9031,#7068,#7069);
#5960=AXIS2_PLACEMENT_3D('',#9034,#7071,#7072);
#5961=AXIS2_PLACEMENT_3D('',#9058,#7073,#7074);
#5962=AXIS2_PLACEMENT_3D('',#9059,#7075,#7076);
#5963=AXIS2_PLACEMENT_3D('',#9060,#7077,#7078);
#5964=AXIS2_PLACEMENT_3D('',#9061,#7079,#7080);
#5965=AXIS2_PLACEMENT_3D('',#9062,#7081,#7082);
#5966=AXIS2_PLACEMENT_3D('',#9063,#7083,#7084);
#5967=AXIS2_PLACEMENT_3D('',#9064,#7085,#7086);
#5968=AXIS2_PLACEMENT_3D('',#9065,#7087,#7088);
#5969=AXIS2_PLACEMENT_3D('',#9066,#7089,#7090);
#5970=AXIS2_PLACEMENT_3D('',#9068,#7091,#7092);
#5971=AXIS2_PLACEMENT_3D('',#9070,#7093,#7094);
#5972=AXIS2_PLACEMENT_3D('',#9071,#7095,#7096);
#5973=AXIS2_PLACEMENT_3D('',#9073,#7097,#7098);
#5974=AXIS2_PLACEMENT_3D('',#9075,#7100,#7101);
#5975=AXIS2_PLACEMENT_3D('',#9077,#7102,#7103);
#5976=AXIS2_PLACEMENT_3D('',#9078,#7104,#7105);
#5977=AXIS2_PLACEMENT_3D('',#9080,#7107,#7108);
#5978=AXIS2_PLACEMENT_3D('',#9082,#7109,#7110);
#5979=AXIS2_PLACEMENT_3D('',#9084,#7111,#7112);
#5980=AXIS2_PLACEMENT_3D('',#9085,#7113,#7114);
#5981=AXIS2_PLACEMENT_3D('',#9087,#7115,#7116);
#5982=AXIS2_PLACEMENT_3D('',#9089,#7118,#7119);
#5983=AXIS2_PLACEMENT_3D('',#9091,#7120,#7121);
#5984=AXIS2_PLACEMENT_3D('',#9092,#7122,#7123);
#5985=AXIS2_PLACEMENT_3D('',#9094,#7125,#7126);
#5986=AXIS2_PLACEMENT_3D('',#9095,#7127,#7128);
#5987=AXIS2_PLACEMENT_3D('',#9096,#7129,#7130);
#5988=AXIS2_PLACEMENT_3D('',#9097,#7131,#7132);
#5989=AXIS2_PLACEMENT_3D('',#9098,#7133,#7134);
#5990=AXIS2_PLACEMENT_3D('',#9099,#7135,#7136);
#5991=AXIS2_PLACEMENT_3D('',#9100,#7137,#7138);
#5992=AXIS2_PLACEMENT_3D('',#9101,#7139,#7140);
#5993=AXIS2_PLACEMENT_3D('',#9110,#7145,#7146);
#5994=AXIS2_PLACEMENT_3D('',#9112,#7147,#7148);
#5995=AXIS2_PLACEMENT_3D('',#9116,#7151,#7152);
#5996=AXIS2_PLACEMENT_3D('',#9122,#7156,#7157);
#5997=AXIS2_PLACEMENT_3D('',#9124,#7159,#7160);
#5998=AXIS2_PLACEMENT_3D('',#9125,#7161,#7162);
#5999=AXIS2_PLACEMENT_3D('',#9126,#7163,#7164);
#6000=AXIS2_PLACEMENT_3D('',#9128,#7165,#7166);
#6001=AXIS2_PLACEMENT_3D('',#9130,#7167,#7168);
#6002=AXIS2_PLACEMENT_3D('',#9131,#7169,#7170);
#6003=AXIS2_PLACEMENT_3D('',#9133,#7171,#7172);
#6004=AXIS2_PLACEMENT_3D('',#9135,#7173,#7174);
#6005=AXIS2_PLACEMENT_3D('',#9136,#7175,#7176);
#6006=AXIS2_PLACEMENT_3D('',#9138,#7178,#7179);
#6007=AXIS2_PLACEMENT_3D('',#9141,#7181,#7182);
#6008=AXIS2_PLACEMENT_3D('',#9142,#7183,#7184);
#6009=AXIS2_PLACEMENT_3D('',#9144,#7185,#7186);
#6010=AXIS2_PLACEMENT_3D('',#9146,#7188,#7189);
#6011=AXIS2_PLACEMENT_3D('',#9147,#7190,#7191);
#6012=AXIS2_PLACEMENT_3D('',#9148,#7192,#7193);
#6013=AXIS2_PLACEMENT_3D('',#9149,#7194,#7195);
#6014=AXIS2_PLACEMENT_3D('',#9151,#7196,#7197);
#6015=AXIS2_PLACEMENT_3D('',#9154,#7199,#7200);
#6016=AXIS2_PLACEMENT_3D('',#9155,#7201,#7202);
#6017=AXIS2_PLACEMENT_3D('',#9157,#7203,#7204);
#6018=AXIS2_PLACEMENT_3D('',#9160,#7206,#7207);
#6019=AXIS2_PLACEMENT_3D('',#9161,#7208,#7209);
#6020=AXIS2_PLACEMENT_3D('',#9165,#7211,#7212);
#6021=AXIS2_PLACEMENT_3D('',#9166,#7213,#7214);
#6022=AXIS2_PLACEMENT_3D('',#9179,#7215,#7216);
#6023=AXIS2_PLACEMENT_3D('',#9220,#7218,#7219);
#6024=AXIS2_PLACEMENT_3D('',#9231,#7220,#7221);
#6025=AXIS2_PLACEMENT_3D('',#9233,#7223,#7224);
#6026=AXIS2_PLACEMENT_3D('',#9242,#7229,#7230);
#6027=AXIS2_PLACEMENT_3D('',#9248,#7234,#7235);
#6028=AXIS2_PLACEMENT_3D('',#9254,#7239,#7240);
#6029=AXIS2_PLACEMENT_3D('',#9256,#7241,#7242);
#6030=AXIS2_PLACEMENT_3D('',#9257,#7243,#7244);
#6031=AXIS2_PLACEMENT_3D('',#9258,#7245,#7246);
#6032=AXIS2_PLACEMENT_3D('',#9259,#7247,#7248);
#6033=AXIS2_PLACEMENT_3D('',#9260,#7249,#7250);
#6034=AXIS2_PLACEMENT_3D('',#9269,#7255,#7256);
#6035=AXIS2_PLACEMENT_3D('',#9278,#7261,#7262);
#6036=AXIS2_PLACEMENT_3D('',#9280,#7263,#7264);
#6037=AXIS2_PLACEMENT_3D('',#9282,#7265,#7266);
#6038=AXIS2_PLACEMENT_3D('',#9286,#7268,#7269);
#6039=AXIS2_PLACEMENT_3D('',#9290,#7271,#7272);
#6040=AXIS2_PLACEMENT_3D('',#9294,#7274,#7275);
#6041=AXIS2_PLACEMENT_3D('',#9297,#7277,#7278);
#6042=AXIS2_PLACEMENT_3D('',#9298,#7279,#7280);
#6043=AXIS2_PLACEMENT_3D('',#9299,#7281,#7282);
#6044=AXIS2_PLACEMENT_3D('',#9301,#7283,#7284);
#6045=AXIS2_PLACEMENT_3D('',#9303,#7286,#7287);
#6046=AXIS2_PLACEMENT_3D('',#9307,#7290,#7291);
#6047=AXIS2_PLACEMENT_3D('',#9313,#7295,#7296);
#6048=AXIS2_PLACEMENT_3D('',#9315,#7297,#7298);
#6049=AXIS2_PLACEMENT_3D('',#9317,#7300,#7301);
#6050=AXIS2_PLACEMENT_3D('',#9321,#7304,#7305);
#6051=AXIS2_PLACEMENT_3D('',#9327,#7309,#7310);
#6052=AXIS2_PLACEMENT_3D('',#9329,#7311,#7312);
#6053=AXIS2_PLACEMENT_3D('',#9330,#7313,#7314);
#6054=AXIS2_PLACEMENT_3D('',#9331,#7315,#7316);
#6055=AXIS2_PLACEMENT_3D('',#9332,#7317,#7318);
#6056=AXIS2_PLACEMENT_3D('',#9333,#7319,#7320);
#6057=AXIS2_PLACEMENT_3D('',#9334,#7321,#7322);
#6058=AXIS2_PLACEMENT_3D('',#9335,#7323,#7324);
#6059=AXIS2_PLACEMENT_3D('',#9337,#7326,#7327);
#6060=AXIS2_PLACEMENT_3D('',#9340,#7329,#7330);
#6061=AXIS2_PLACEMENT_3D('',#9341,#7331,#7332);
#6062=AXIS2_PLACEMENT_3D('',#9342,#7333,#7334);
#6063=AXIS2_PLACEMENT_3D('',#9343,#7335,#7336);
#6064=AXIS2_PLACEMENT_3D('',#9345,#7337,#7338);
#6065=AXIS2_PLACEMENT_3D('',#9348,#7340,#7341);
#6066=AXIS2_PLACEMENT_3D('',#9349,#7342,#7343);
#6067=AXIS2_PLACEMENT_3D('',#9351,#7344,#7345);
#6068=AXIS2_PLACEMENT_3D('',#9354,#7347,#7348);
#6069=AXIS2_PLACEMENT_3D('',#9355,#7349,#7350);
#6070=AXIS2_PLACEMENT_3D('',#9356,#7351,#7352);
#6071=AXIS2_PLACEMENT_3D('',#9357,#7353,#7354);
#6072=AXIS2_PLACEMENT_3D('',#9358,#7355,#7356);
#6073=AXIS2_PLACEMENT_3D('',#9362,#7358,#7359);
#6074=AXIS2_PLACEMENT_3D('',#9363,#7360,#7361);
#6075=AXIS2_PLACEMENT_3D('',#9376,#7362,#7363);
#6076=AXIS2_PLACEMENT_3D('',#9417,#7365,#7366);
#6077=AXIS2_PLACEMENT_3D('',#9428,#7367,#7368);
#6078=AXIS2_PLACEMENT_3D('',#9430,#7370,#7371);
#6079=AXIS2_PLACEMENT_3D('',#9432,#7372,#7373);
#6080=AXIS2_PLACEMENT_3D('',#9435,#7375,#7376);
#6081=AXIS2_PLACEMENT_3D('',#9436,#7377,#7378);
#6082=AXIS2_PLACEMENT_3D('',#9438,#7379,#7380);
#6083=AXIS2_PLACEMENT_3D('',#9441,#7382,#7383);
#6084=AXIS2_PLACEMENT_3D('',#9442,#7384,#7385);
#6085=AXIS2_PLACEMENT_3D('',#9443,#7386,#7387);
#6086=AXIS2_PLACEMENT_3D('',#9444,#7388,#7389);
#6087=AXIS2_PLACEMENT_3D('',#9445,#7390,#7391);
#6088=AXIS2_PLACEMENT_3D('',#9447,#7392,#7393);
#6089=AXIS2_PLACEMENT_3D('',#9450,#7395,#7396);
#6090=AXIS2_PLACEMENT_3D('',#9451,#7397,#7398);
#6091=AXIS2_PLACEMENT_3D('',#9452,#7399,#7400);
#6092=AXIS2_PLACEMENT_3D('',#9454,#7401,#7402);
#6093=AXIS2_PLACEMENT_3D('',#9457,#7404,#7405);
#6094=AXIS2_PLACEMENT_3D('',#9458,#7406,#7407);
#6095=AXIS2_PLACEMENT_3D('',#9460,#7408,#7409);
#6096=AXIS2_PLACEMENT_3D('',#9463,#7411,#7412);
#6097=AXIS2_PLACEMENT_3D('',#9464,#7413,#7414);
#6098=AXIS2_PLACEMENT_3D('',#9466,#7415,#7416);
#6099=AXIS2_PLACEMENT_3D('',#9468,#7417,#7418);
#6100=AXIS2_PLACEMENT_3D('',#9469,#7419,#7420);
#6101=AXIS2_PLACEMENT_3D('',#9471,#7421,#7422);
#6102=AXIS2_PLACEMENT_3D('',#9473,#7424,#7425);
#6103=AXIS2_PLACEMENT_3D('',#9475,#7426,#7427);
#6104=AXIS2_PLACEMENT_3D('',#9477,#7428,#7429);
#6105=AXIS2_PLACEMENT_3D('',#9478,#7430,#7431);
#6106=AXIS2_PLACEMENT_3D('',#9480,#7433,#7434);
#6107=AXIS2_PLACEMENT_3D('',#9483,#7436,#7437);
#6108=AXIS2_PLACEMENT_3D('',#9484,#7438,#7439);
#6109=AXIS2_PLACEMENT_3D('',#9485,#7440,#7441);
#6110=AXIS2_PLACEMENT_3D('',#9486,#7442,#7443);
#6111=AXIS2_PLACEMENT_3D('',#9487,#7444,#7445);
#6112=AXIS2_PLACEMENT_3D('',#9489,#7446,#7447);
#6113=AXIS2_PLACEMENT_3D('',#9492,#7449,#7450);
#6114=AXIS2_PLACEMENT_3D('',#9493,#7451,#7452);
#6115=AXIS2_PLACEMENT_3D('',#9495,#7453,#7454);
#6116=AXIS2_PLACEMENT_3D('',#9498,#7456,#7457);
#6117=AXIS2_PLACEMENT_3D('',#9499,#7458,#7459);
#6118=AXIS2_PLACEMENT_3D('',#9500,#7460,#7461);
#6119=AXIS2_PLACEMENT_3D('',#9501,#7462,#7463);
#6120=AXIS2_PLACEMENT_3D('',#9502,#7464,#7465);
#6121=AXIS2_PLACEMENT_3D('',#9504,#7466,#7467);
#6122=AXIS2_PLACEMENT_3D('',#9507,#7469,#7470);
#6123=AXIS2_PLACEMENT_3D('',#9508,#7471,#7472);
#6124=AXIS2_PLACEMENT_3D('',#9510,#7473,#7474);
#6125=AXIS2_PLACEMENT_3D('',#9513,#7476,#7477);
#6126=AXIS2_PLACEMENT_3D('',#9514,#7478,#7479);
#6127=AXIS2_PLACEMENT_3D('',#9515,#7480,#7481);
#6128=AXIS2_PLACEMENT_3D('',#9516,#7482,#7483);
#6129=AXIS2_PLACEMENT_3D('',#9517,#7484,#7485);
#6130=AXIS2_PLACEMENT_3D('',#9526,#7490,#7491);
#6131=AXIS2_PLACEMENT_3D('',#9530,#7493,#7494);
#6132=AXIS2_PLACEMENT_3D('',#9531,#7495,#7496);
#6133=AXIS2_PLACEMENT_3D('',#9532,#7497,#7498);
#6134=AXIS2_PLACEMENT_3D('',#9538,#7502,#7503);
#6135=AXIS2_PLACEMENT_3D('',#9539,#7504,#7505);
#6136=AXIS2_PLACEMENT_3D('',#9540,#7506,#7507);
#6137=AXIS2_PLACEMENT_3D('',#9541,#7508,#7509);
#6138=AXIS2_PLACEMENT_3D('',#9545,#7511,#7512);
#6139=AXIS2_PLACEMENT_3D('',#9547,#7514,#7515);
#6140=AXIS2_PLACEMENT_3D('',#9551,#7518,#7519);
#6141=AXIS2_PLACEMENT_3D('',#9552,#7520,#7521);
#6142=AXIS2_PLACEMENT_3D('',#9558,#7525,#7526);
#6143=AXIS2_PLACEMENT_3D('',#9561,#7528,#7529);
#6144=AXIS2_PLACEMENT_3D('',#9562,#7530,#7531);
#6145=AXIS2_PLACEMENT_3D('',#9568,#7535,#7536);
#6146=AXIS2_PLACEMENT_3D('',#9569,#7537,#7538);
#6147=AXIS2_PLACEMENT_3D('',#9570,#7539,#7540);
#6148=AXIS2_PLACEMENT_3D('',#9571,#7541,#7542);
#6149=AXIS2_PLACEMENT_3D('',#9573,#7544,#7545);
#6150=AXIS2_PLACEMENT_3D('',#9574,#7546,#7547);
#6151=AXIS2_PLACEMENT_3D('',#9575,#7548,#7549);
#6152=AXIS2_PLACEMENT_3D('',#9576,#7550,#7551);
#6153=AXIS2_PLACEMENT_3D('',#9585,#7556,#7557);
#6154=AXIS2_PLACEMENT_3D('',#9591,#7561,#7562);
#6155=AXIS2_PLACEMENT_3D('',#9597,#7566,#7567);
#6156=AXIS2_PLACEMENT_3D('',#9603,#7571,#7572);
#6157=AXIS2_PLACEMENT_3D('',#9609,#7576,#7577);
#6158=AXIS2_PLACEMENT_3D('',#9612,#7580,#7581);
#6159=AXIS2_PLACEMENT_3D('',#9613,#7582,#7583);
#6160=AXIS2_PLACEMENT_3D('',#9615,#7584,#7585);
#6161=AXIS2_PLACEMENT_3D('',#9616,#7586,#7587);
#6162=AXIS2_PLACEMENT_3D('',#9618,#7588,#7589);
#6163=AXIS2_PLACEMENT_3D('',#9620,#7591,#7592);
#6164=AXIS2_PLACEMENT_3D('',#9622,#7593,#7594);
#6165=AXIS2_PLACEMENT_3D('',#9624,#7596,#7597);
#6166=AXIS2_PLACEMENT_3D('',#9626,#7598,#7599);
#6167=AXIS2_PLACEMENT_3D('',#9628,#7601,#7602);
#6168=AXIS2_PLACEMENT_3D('',#9629,#7603,#7604);
#6169=AXIS2_PLACEMENT_3D('',#9630,#7605,#7606);
#6170=AXIS2_PLACEMENT_3D('',#9639,#7611,#7612);
#6171=AXIS2_PLACEMENT_3D('',#9645,#7616,#7617);
#6172=AXIS2_PLACEMENT_3D('',#9651,#7621,#7622);
#6173=AXIS2_PLACEMENT_3D('',#9657,#7626,#7627);
#6174=AXIS2_PLACEMENT_3D('',#9663,#7631,#7632);
#6175=AXIS2_PLACEMENT_3D('',#9666,#7635,#7636);
#6176=AXIS2_PLACEMENT_3D('',#9667,#7637,#7638);
#6177=AXIS2_PLACEMENT_3D('',#9668,#7639,#7640);
#6178=AXIS2_PLACEMENT_3D('',#9670,#7641,#7642);
#6179=AXIS2_PLACEMENT_3D('',#9671,#7643,#7644);
#6180=AXIS2_PLACEMENT_3D('',#9673,#7645,#7646);
#6181=AXIS2_PLACEMENT_3D('',#9674,#7647,#7648);
#6182=AXIS2_PLACEMENT_3D('',#9676,#7649,#7650);
#6183=AXIS2_PLACEMENT_3D('',#9678,#7652,#7653);
#6184=AXIS2_PLACEMENT_3D('',#9680,#7654,#7655);
#6185=AXIS2_PLACEMENT_3D('',#9682,#7657,#7658);
#6186=AXIS2_PLACEMENT_3D('',#9684,#7659,#7660);
#6187=AXIS2_PLACEMENT_3D('',#9686,#7662,#7663);
#6188=AXIS2_PLACEMENT_3D('',#9688,#7664,#7665);
#6189=AXIS2_PLACEMENT_3D('',#9689,#7666,#7667);
#6190=AXIS2_PLACEMENT_3D('',#9691,#7668,#7669);
#6191=AXIS2_PLACEMENT_3D('',#9693,#7671,#7672);
#6192=AXIS2_PLACEMENT_3D('',#9695,#7674,#7675);
#6193=AXIS2_PLACEMENT_3D('',#9696,#7676,#7677);
#6194=AXIS2_PLACEMENT_3D('',#9697,#7678,#7679);
#6195=AXIS2_PLACEMENT_3D('',#9700,#7680,#7681);
#6196=AXIS2_PLACEMENT_3D('',#9701,#7682,#7683);
#6197=AXIS2_PLACEMENT_3D('',#9703,#7684,#7685);
#6198=AXIS2_PLACEMENT_3D('',#9705,#7686,#7687);
#6199=AXIS2_PLACEMENT_3D('',#9706,#7688,#7689);
#6200=AXIS2_PLACEMENT_3D('',#9707,#7690,#7691);
#6201=AXIS2_PLACEMENT_3D('',#9710,#7693,#7694);
#6202=AXIS2_PLACEMENT_3D('',#9711,#7695,#7696);
#6203=AXIS2_PLACEMENT_3D('',#9713,#7697,#7698);
#6204=AXIS2_PLACEMENT_3D('',#9716,#7700,#7701);
#6205=AXIS2_PLACEMENT_3D('',#9717,#7702,#7703);
#6206=AXIS2_PLACEMENT_3D('',#9720,#7705,#7706);
#6207=AXIS2_PLACEMENT_3D('',#9721,#7707,#7708);
#6208=AXIS2_PLACEMENT_3D('',#9722,#7709,#7710);
#6209=AXIS2_PLACEMENT_3D('',#9724,#7711,#7712);
#6210=AXIS2_PLACEMENT_3D('',#9726,#7714,#7715);
#6211=AXIS2_PLACEMENT_3D('',#9728,#7716,#7717);
#6212=AXIS2_PLACEMENT_3D('',#9729,#7718,#7719);
#6213=AXIS2_PLACEMENT_3D('',#9731,#7721,#7722);
#6214=AXIS2_PLACEMENT_3D('',#9732,#7723,#7724);
#6215=AXIS2_PLACEMENT_3D('',#9735,#7725,#7726);
#6216=AXIS2_PLACEMENT_3D('',#9736,#7727,#7728);
#6217=AXIS2_PLACEMENT_3D('',#9738,#7729,#7730);
#6218=AXIS2_PLACEMENT_3D('',#9740,#7731,#7732);
#6219=AXIS2_PLACEMENT_3D('',#9741,#7733,#7734);
#6220=AXIS2_PLACEMENT_3D('',#9742,#7735,#7736);
#6221=AXIS2_PLACEMENT_3D('',#9744,#7737,#7738);
#6222=AXIS2_PLACEMENT_3D('',#9746,#7740,#7741);
#6223=AXIS2_PLACEMENT_3D('',#9748,#7742,#7743);
#6224=AXIS2_PLACEMENT_3D('',#9750,#7744,#7745);
#6225=AXIS2_PLACEMENT_3D('',#9751,#7746,#7747);
#6226=AXIS2_PLACEMENT_3D('',#9753,#7748,#7749);
#6227=AXIS2_PLACEMENT_3D('',#9755,#7751,#7752);
#6228=AXIS2_PLACEMENT_3D('',#9757,#7753,#7754);
#6229=AXIS2_PLACEMENT_3D('',#9759,#7756,#7757);
#6230=AXIS2_PLACEMENT_3D('',#9761,#7758,#7759);
#6231=AXIS2_PLACEMENT_3D('',#9763,#7761,#7762);
#6232=AXIS2_PLACEMENT_3D('',#9764,#7763,#7764);
#6233=AXIS2_PLACEMENT_3D('',#9766,#7766,#7767);
#6234=AXIS2_PLACEMENT_3D('',#9767,#7768,#7769);
#6235=AXIS2_PLACEMENT_3D('',#9770,#7770,#7771);
#6236=AXIS2_PLACEMENT_3D('',#9771,#7772,#7773);
#6237=AXIS2_PLACEMENT_3D('',#9774,#7774,#7775);
#6238=AXIS2_PLACEMENT_3D('',#9775,#7776,#7777);
#6239=AXIS2_PLACEMENT_3D('',#9778,#7778,#7779);
#6240=AXIS2_PLACEMENT_3D('',#9779,#7780,#7781);
#6241=AXIS2_PLACEMENT_3D('',#9782,#7782,#7783);
#6242=AXIS2_PLACEMENT_3D('',#9783,#7784,#7785);
#6243=AXIS2_PLACEMENT_3D('',#9786,#7786,#7787);
#6244=AXIS2_PLACEMENT_3D('',#9787,#7788,#7789);
#6245=AXIS2_PLACEMENT_3D('',#9790,#7790,#7791);
#6246=AXIS2_PLACEMENT_3D('',#9791,#7792,#7793);
#6247=AXIS2_PLACEMENT_3D('',#9794,#7794,#7795);
#6248=AXIS2_PLACEMENT_3D('',#9795,#7796,#7797);
#6249=AXIS2_PLACEMENT_3D('',#9798,#7798,#7799);
#6250=AXIS2_PLACEMENT_3D('',#9799,#7800,#7801);
#6251=AXIS2_PLACEMENT_3D('',#9800,#7802,#7803);
#6252=AXIS2_PLACEMENT_3D('',#9826,#7804,#7805);
#6253=AXIS2_PLACEMENT_3D('',#9850,#7806,#7807);
#6254=AXIS2_PLACEMENT_3D('',#9851,#7808,#7809);
#6255=AXIS2_PLACEMENT_3D('',#9853,#7810,#7811);
#6256=AXIS2_PLACEMENT_3D('',#9878,#7812,#7813);
#6257=AXIS2_PLACEMENT_3D('',#9903,#7814,#7815);
#6258=AXIS2_PLACEMENT_3D('',#9919,#7817,#7818);
#6259=AXIS2_PLACEMENT_3D('',#9934,#7819,#7820);
#6260=AXIS2_PLACEMENT_3D('',#9959,#7821,#7822);
#6261=AXIS2_PLACEMENT_3D('',#9984,#7823,#7824);
#6262=AXIS2_PLACEMENT_3D('',#10009,#7825,#7826);
#6263=AXIS2_PLACEMENT_3D('',#10033,#7827,#7828);
#6264=AXIS2_PLACEMENT_3D('',#10034,#7829,#7830);
#6265=AXIS2_PLACEMENT_3D('',#10036,#7831,#7832);
#6266=AXIS2_PLACEMENT_3D('',#10037,#7833,#7834);
#6267=AXIS2_PLACEMENT_3D('',#10038,#7835,#7836);
#6268=AXIS2_PLACEMENT_3D('',#10062,#7837,#7838);
#6269=AXIS2_PLACEMENT_3D('',#10063,#7839,#7840);
#6270=AXIS2_PLACEMENT_3D('',#10065,#7841,#7842);
#6271=AXIS2_PLACEMENT_3D('',#10066,#7843,#7844);
#6272=AXIS2_PLACEMENT_3D('',#10067,#7845,#7846);
#6273=AXIS2_PLACEMENT_3D('',#10091,#7847,#7848);
#6274=AXIS2_PLACEMENT_3D('',#10092,#7849,#7850);
#6275=AXIS2_PLACEMENT_3D('',#10094,#7851,#7852);
#6276=AXIS2_PLACEMENT_3D('',#10095,#7853,#7854);
#6277=AXIS2_PLACEMENT_3D('',#10096,#7855,#7856);
#6278=AXIS2_PLACEMENT_3D('',#10111,#7857,#7858);
#6279=AXIS2_PLACEMENT_3D('',#10124,#7859,#7860);
#6280=AXIS2_PLACEMENT_3D('',#10126,#7861,#7862);
#6281=AXIS2_PLACEMENT_3D('',#10127,#7863,#7864);
#6282=AXIS2_PLACEMENT_3D('',#10128,#7865,#7866);
#6283=AXIS2_PLACEMENT_3D('',#10152,#7867,#7868);
#6284=AXIS2_PLACEMENT_3D('',#10153,#7869,#7870);
#6285=AXIS2_PLACEMENT_3D('',#10155,#7871,#7872);
#6286=AXIS2_PLACEMENT_3D('',#10156,#7873,#7874);
#6287=AXIS2_PLACEMENT_3D('',#10157,#7875,#7876);
#6288=AXIS2_PLACEMENT_3D('',#10181,#7877,#7878);
#6289=AXIS2_PLACEMENT_3D('',#10182,#7879,#7880);
#6290=AXIS2_PLACEMENT_3D('',#10184,#7881,#7882);
#6291=AXIS2_PLACEMENT_3D('',#10185,#7883,#7884);
#6292=AXIS2_PLACEMENT_3D('',#10186,#7885,#7886);
#6293=AXIS2_PLACEMENT_3D('',#10210,#7887,#7888);
#6294=AXIS2_PLACEMENT_3D('',#10211,#7889,#7890);
#6295=AXIS2_PLACEMENT_3D('',#10213,#7891,#7892);
#6296=AXIS2_PLACEMENT_3D('',#10216,#7894,#7895);
#6297=AXIS2_PLACEMENT_3D('',#10240,#7896,#7897);
#6298=AXIS2_PLACEMENT_3D('',#10241,#7898,#7899);
#6299=AXIS2_PLACEMENT_3D('',#10242,#7900,#7901);
#6300=AXIS2_PLACEMENT_3D('',#10243,#7902,#7903);
#6301=AXIS2_PLACEMENT_3D('',#10244,#7904,#7905);
#6302=AXIS2_PLACEMENT_3D('',#10245,#7906,#7907);
#6303=AXIS2_PLACEMENT_3D('',#10246,#7908,#7909);
#6304=AXIS2_PLACEMENT_3D('',#10247,#7910,#7911);
#6305=AXIS2_PLACEMENT_3D('',#10248,#7912,#7913);
#6306=AXIS2_PLACEMENT_3D('',#10250,#7914,#7915);
#6307=AXIS2_PLACEMENT_3D('',#10252,#7916,#7917);
#6308=AXIS2_PLACEMENT_3D('',#10253,#7918,#7919);
#6309=AXIS2_PLACEMENT_3D('',#10255,#7920,#7921);
#6310=AXIS2_PLACEMENT_3D('',#10257,#7923,#7924);
#6311=AXIS2_PLACEMENT_3D('',#10259,#7925,#7926);
#6312=AXIS2_PLACEMENT_3D('',#10260,#7927,#7928);
#6313=AXIS2_PLACEMENT_3D('',#10262,#7930,#7931);
#6314=AXIS2_PLACEMENT_3D('',#10264,#7932,#7933);
#6315=AXIS2_PLACEMENT_3D('',#10266,#7934,#7935);
#6316=AXIS2_PLACEMENT_3D('',#10267,#7936,#7937);
#6317=AXIS2_PLACEMENT_3D('',#10269,#7938,#7939);
#6318=AXIS2_PLACEMENT_3D('',#10271,#7941,#7942);
#6319=AXIS2_PLACEMENT_3D('',#10273,#7943,#7944);
#6320=AXIS2_PLACEMENT_3D('',#10274,#7945,#7946);
#6321=AXIS2_PLACEMENT_3D('',#10276,#7948,#7949);
#6322=AXIS2_PLACEMENT_3D('',#10277,#7950,#7951);
#6323=AXIS2_PLACEMENT_3D('',#10278,#7952,#7953);
#6324=AXIS2_PLACEMENT_3D('',#10279,#7954,#7955);
#6325=AXIS2_PLACEMENT_3D('',#10280,#7956,#7957);
#6326=AXIS2_PLACEMENT_3D('',#10281,#7958,#7959);
#6327=AXIS2_PLACEMENT_3D('',#10282,#7960,#7961);
#6328=AXIS2_PLACEMENT_3D('',#10284,#7962,#7963);
#6329=AXIS2_PLACEMENT_3D('',#10285,#7964,#7965);
#6330=AXIS2_PLACEMENT_3D('',#10287,#7966,#7967);
#6331=AXIS2_PLACEMENT_3D('',#10289,#7969,#7970);
#6332=AXIS2_PLACEMENT_3D('',#10291,#7971,#7972);
#6333=AXIS2_PLACEMENT_3D('',#10293,#7974,#7975);
#6334=AXIS2_PLACEMENT_3D('',#10295,#7976,#7977);
#6335=AXIS2_PLACEMENT_3D('',#10297,#7979,#7980);
#6336=AXIS2_PLACEMENT_3D('',#10299,#7981,#7982);
#6337=AXIS2_PLACEMENT_3D('',#10300,#7983,#7984);
#6338=AXIS2_PLACEMENT_3D('',#10302,#7985,#7986);
#6339=AXIS2_PLACEMENT_3D('',#10304,#7988,#7989);
#6340=AXIS2_PLACEMENT_3D('',#10306,#7990,#7991);
#6341=AXIS2_PLACEMENT_3D('',#10308,#7993,#7994);
#6342=AXIS2_PLACEMENT_3D('',#10310,#7995,#7996);
#6343=AXIS2_PLACEMENT_3D('',#10312,#7998,#7999);
#6344=AXIS2_PLACEMENT_3D('',#10313,#8000,#8001);
#6345=AXIS2_PLACEMENT_3D('',#10322,#8006,#8007);
#6346=AXIS2_PLACEMENT_3D('',#10328,#8011,#8012);
#6347=AXIS2_PLACEMENT_3D('',#10334,#8016,#8017);
#6348=AXIS2_PLACEMENT_3D('',#10340,#8021,#8022);
#6349=AXIS2_PLACEMENT_3D('',#10346,#8026,#8027);
#6350=AXIS2_PLACEMENT_3D('',#10349,#8030,#8031);
#6351=AXIS2_PLACEMENT_3D('',#10350,#8032,#8033);
#6352=AXIS2_PLACEMENT_3D('',#10351,#8034,#8035);
#6353=AXIS2_PLACEMENT_3D('',#10352,#8036,#8037);
#6354=AXIS2_PLACEMENT_3D('',#10353,#8038,#8039);
#6355=AXIS2_PLACEMENT_3D('',#10354,#8040,#8041);
#6356=AXIS2_PLACEMENT_3D('',#10355,#8042,#8043);
#6357=AXIS2_PLACEMENT_3D('',#10356,#8044,#8045);
#6358=AXIS2_PLACEMENT_3D('',#10357,#8046,#8047);
#6359=AXIS2_PLACEMENT_3D('',#10358,#8048,#8049);
#6360=AXIS2_PLACEMENT_3D('',#10359,#8050,#8051);
#6361=AXIS2_PLACEMENT_3D('',#10360,#8052,#8053);
#6362=AXIS2_PLACEMENT_3D('',#10361,#8054,#8055);
#6363=AXIS2_PLACEMENT_3D('',#10362,#8056,#8057);
#6364=AXIS2_PLACEMENT_3D('',#10363,#8058,#8059);
#6365=AXIS2_PLACEMENT_3D('',#10364,#8060,#8061);
#6366=AXIS2_PLACEMENT_3D('',#10365,#8062,#8063);
#6367=AXIS2_PLACEMENT_3D('',#10366,#8064,#8065);
#6368=AXIS2_PLACEMENT_3D('',#10367,#8066,#8067);
#6369=AXIS2_PLACEMENT_3D('',#10368,#8068,#8069);
#6370=AXIS2_PLACEMENT_3D('',#10369,#8070,#8071);
#6371=AXIS2_PLACEMENT_3D('',#10370,#8072,#8073);
#6372=AXIS2_PLACEMENT_3D('',#10371,#8074,#8075);
#6373=AXIS2_PLACEMENT_3D('',#10372,#8076,#8077);
#6374=AXIS2_PLACEMENT_3D('',#10373,#8078,#8079);
#6375=AXIS2_PLACEMENT_3D('',#10374,#8080,#8081);
#6376=AXIS2_PLACEMENT_3D('',#10375,#8082,#8083);
#6377=AXIS2_PLACEMENT_3D('',#10376,#8084,#8085);
#6378=AXIS2_PLACEMENT_3D('',#10377,#8086,#8087);
#6379=AXIS2_PLACEMENT_3D('',#10378,#8088,#8089);
#6380=AXIS2_PLACEMENT_3D('',#10379,#8090,#8091);
#6381=AXIS2_PLACEMENT_3D('',#10380,#8092,#8093);
#6382=AXIS2_PLACEMENT_3D('',#10381,#8094,#8095);
#6383=AXIS2_PLACEMENT_3D('',#10382,#8096,#8097);
#6384=AXIS2_PLACEMENT_3D('',#10383,#8098,#8099);
#6385=AXIS2_PLACEMENT_3D('',#10384,#8100,#8101);
#6386=AXIS2_PLACEMENT_3D('',#10385,#8102,#8103);
#6387=AXIS2_PLACEMENT_3D('',#10386,#8104,#8105);
#6388=AXIS2_PLACEMENT_3D('',#10387,#8106,#8107);
#6389=AXIS2_PLACEMENT_3D('',#10388,#8108,#8109);
#6390=AXIS2_PLACEMENT_3D('',#10389,#8110,#8111);
#6391=AXIS2_PLACEMENT_3D('',#10390,#8112,#8113);
#6392=AXIS2_PLACEMENT_3D('',#10391,#8114,#8115);
#6393=AXIS2_PLACEMENT_3D('',#10392,#8116,#8117);
#6394=AXIS2_PLACEMENT_3D('',#10394,#8118,#8119);
#6395=AXIS2_PLACEMENT_3D('',#10397,#8121,#8122);
#6396=AXIS2_PLACEMENT_3D('',#10398,#8123,#8124);
#6397=AXIS2_PLACEMENT_3D('',#10400,#8125,#8126);
#6398=AXIS2_PLACEMENT_3D('',#10401,#8127,#8128);
#6399=AXIS2_PLACEMENT_3D('',#10404,#8130,#8131);
#6400=AXIS2_PLACEMENT_3D('',#10405,#8132,#8133);
#6401=AXIS2_PLACEMENT_3D('',#10407,#8134,#8135);
#6402=AXIS2_PLACEMENT_3D('',#10410,#8137,#8138);
#6403=AXIS2_PLACEMENT_3D('',#10411,#8139,#8140);
#6404=AXIS2_PLACEMENT_3D('',#10412,#8141,#8142);
#6405=AXIS2_PLACEMENT_3D('',#10413,#8143,#8144);
#6406=AXIS2_PLACEMENT_3D('',#10414,#8145,#8146);
#6407=AXIS2_PLACEMENT_3D('',#10416,#8147,#8148);
#6408=AXIS2_PLACEMENT_3D('',#10419,#8150,#8151);
#6409=AXIS2_PLACEMENT_3D('',#10420,#8152,#8153);
#6410=AXIS2_PLACEMENT_3D('',#10422,#8154,#8155);
#6411=AXIS2_PLACEMENT_3D('',#10425,#8157,#8158);
#6412=AXIS2_PLACEMENT_3D('',#10426,#8159,#8160);
#6413=AXIS2_PLACEMENT_3D('',#10427,#8161,#8162);
#6414=AXIS2_PLACEMENT_3D('',#10428,#8163,#8164);
#6415=AXIS2_PLACEMENT_3D('',#10429,#8165,#8166);
#6416=AXIS2_PLACEMENT_3D('',#10430,#8167,#8168);
#6417=AXIS2_PLACEMENT_3D('',#10431,#8169,#8170);
#6418=AXIS2_PLACEMENT_3D('',#10432,#8171,#8172);
#6419=DIRECTION('axis',(0.,0.,1.));
#6420=DIRECTION('refdir',(1.,0.,0.));
#6421=DIRECTION('axis',(0.,0.,1.));
#6422=DIRECTION('refdir',(1.,0.,0.));
#6423=DIRECTION('axis',(0.,0.,1.));
#6424=DIRECTION('refdir',(1.,0.,0.));
#6425=DIRECTION('center_axis',(0.,0.,1.));
#6426=DIRECTION('ref_axis',(1.,0.,0.));
#6427=DIRECTION('center_axis',(0.,0.,1.));
#6428=DIRECTION('ref_axis',(1.,0.,0.));
#6429=DIRECTION('',(0.,0.,1.));
#6430=DIRECTION('center_axis',(0.,0.,-1.));
#6431=DIRECTION('ref_axis',(1.,0.,0.));
#6432=DIRECTION('center_axis',(0.,0.,1.));
#6433=DIRECTION('ref_axis',(1.,0.,0.));
#6434=DIRECTION('center_axis',(0.,0.,1.));
#6435=DIRECTION('ref_axis',(1.,0.,0.));
#6436=DIRECTION('',(0.,0.,1.));
#6437=DIRECTION('center_axis',(0.,0.,-1.));
#6438=DIRECTION('ref_axis',(1.,0.,0.));
#6439=DIRECTION('center_axis',(0.,0.,1.));
#6440=DIRECTION('ref_axis',(1.,0.,0.));
#6441=DIRECTION('center_axis',(0.,0.,1.));
#6442=DIRECTION('ref_axis',(1.,0.,0.));
#6443=DIRECTION('',(0.,0.,1.));
#6444=DIRECTION('center_axis',(0.,0.,-1.));
#6445=DIRECTION('ref_axis',(1.,0.,0.));
#6446=DIRECTION('center_axis',(0.,0.,1.));
#6447=DIRECTION('ref_axis',(1.,0.,0.));
#6448=DIRECTION('center_axis',(0.,0.,1.));
#6449=DIRECTION('ref_axis',(1.,0.,0.));
#6450=DIRECTION('',(0.,0.,1.));
#6451=DIRECTION('center_axis',(0.,0.,-1.));
#6452=DIRECTION('ref_axis',(1.,0.,0.));
#6453=DIRECTION('center_axis',(0.,1.,0.));
#6454=DIRECTION('ref_axis',(-1.,0.,0.));
#6455=DIRECTION('',(-1.,0.,0.));
#6456=DIRECTION('',(0.,0.,1.));
#6457=DIRECTION('',(-1.,0.,0.));
#6458=DIRECTION('',(0.,0.,1.));
#6459=DIRECTION('center_axis',(1.,0.,0.));
#6460=DIRECTION('ref_axis',(0.,1.,0.));
#6461=DIRECTION('',(0.,1.,0.));
#6462=DIRECTION('',(0.,1.,0.));
#6463=DIRECTION('',(0.,0.,1.));
#6464=DIRECTION('center_axis',(0.,-1.,0.));
#6465=DIRECTION('ref_axis',(1.,0.,0.));
#6466=DIRECTION('',(1.,0.,0.));
#6467=DIRECTION('',(1.,0.,0.));
#6468=DIRECTION('',(0.,0.,1.));
#6469=DIRECTION('center_axis',(-1.,0.,0.));
#6470=DIRECTION('ref_axis',(0.,-1.,0.));
#6471=DIRECTION('',(0.,-1.,0.));
#6472=DIRECTION('',(0.,-1.,0.));
#6473=DIRECTION('center_axis',(0.,0.,1.));
#6474=DIRECTION('ref_axis',(1.,0.,0.));
#6475=DIRECTION('center_axis',(0.,0.,1.));
#6476=DIRECTION('ref_axis',(1.,0.,0.));
#6477=DIRECTION('axis',(0.,0.,1.));
#6478=DIRECTION('refdir',(1.,0.,0.));
#6479=DIRECTION('center_axis',(0.,1.,0.));
#6480=DIRECTION('ref_axis',(-1.,0.,0.));
#6481=DIRECTION('',(-1.,0.,0.));
#6482=DIRECTION('',(0.,0.,1.));
#6483=DIRECTION('',(-1.,0.,0.));
#6484=DIRECTION('',(0.,0.,1.));
#6485=DIRECTION('center_axis',(1.,0.,0.));
#6486=DIRECTION('ref_axis',(0.,1.,0.));
#6487=DIRECTION('',(0.,1.,0.));
#6488=DIRECTION('',(0.,1.,0.));
#6489=DIRECTION('',(0.,0.,1.));
#6490=DIRECTION('center_axis',(0.,-1.,0.));
#6491=DIRECTION('ref_axis',(1.,0.,0.));
#6492=DIRECTION('',(1.,0.,0.));
#6493=DIRECTION('',(1.,0.,0.));
#6494=DIRECTION('',(0.,0.,1.));
#6495=DIRECTION('center_axis',(-1.,0.,0.));
#6496=DIRECTION('ref_axis',(0.,-1.,0.));
#6497=DIRECTION('',(0.,-1.,0.));
#6498=DIRECTION('',(0.,-1.,0.));
#6499=DIRECTION('center_axis',(0.,0.,1.));
#6500=DIRECTION('ref_axis',(1.,0.,0.));
#6501=DIRECTION('center_axis',(0.,0.,1.));
#6502=DIRECTION('ref_axis',(1.,0.,0.));
#6503=DIRECTION('axis',(0.,0.,1.));
#6504=DIRECTION('refdir',(1.,0.,0.));
#6505=DIRECTION('center_axis',(0.,1.,0.));
#6506=DIRECTION('ref_axis',(-1.,0.,0.));
#6507=DIRECTION('',(-1.,0.,0.));
#6508=DIRECTION('',(0.,0.,1.));
#6509=DIRECTION('',(-1.,0.,0.));
#6510=DIRECTION('',(0.,0.,1.));
#6511=DIRECTION('center_axis',(1.,0.,0.));
#6512=DIRECTION('ref_axis',(0.,1.,0.));
#6513=DIRECTION('',(0.,1.,0.));
#6514=DIRECTION('',(0.,1.,0.));
#6515=DIRECTION('',(0.,0.,1.));
#6516=DIRECTION('center_axis',(0.,-1.,0.));
#6517=DIRECTION('ref_axis',(1.,0.,0.));
#6518=DIRECTION('',(1.,0.,0.));
#6519=DIRECTION('',(1.,0.,0.));
#6520=DIRECTION('',(0.,0.,1.));
#6521=DIRECTION('center_axis',(-1.,0.,0.));
#6522=DIRECTION('ref_axis',(0.,-1.,0.));
#6523=DIRECTION('',(0.,-1.,0.));
#6524=DIRECTION('',(0.,-1.,0.));
#6525=DIRECTION('center_axis',(0.,0.,1.));
#6526=DIRECTION('ref_axis',(1.,0.,0.));
#6527=DIRECTION('center_axis',(0.,0.,1.));
#6528=DIRECTION('ref_axis',(1.,0.,0.));
#6529=DIRECTION('axis',(0.,0.,1.));
#6530=DIRECTION('refdir',(1.,0.,0.));
#6531=DIRECTION('center_axis',(0.,1.,0.));
#6532=DIRECTION('ref_axis',(1.,0.,0.));
#6533=DIRECTION('center_axis',(0.,1.,0.));
#6534=DIRECTION('ref_axis',(1.,0.,0.));
#6535=DIRECTION('',(0.,1.,0.));
#6536=DIRECTION('center_axis',(0.,-1.,0.));
#6537=DIRECTION('ref_axis',(1.,0.,0.));
#6538=DIRECTION('center_axis',(0.,1.,0.));
#6539=DIRECTION('ref_axis',(1.,0.,0.));
#6540=DIRECTION('center_axis',(0.,1.,0.));
#6541=DIRECTION('ref_axis',(1.,0.,0.));
#6542=DIRECTION('',(0.,1.,0.));
#6543=DIRECTION('center_axis',(0.,-1.,0.));
#6544=DIRECTION('ref_axis',(1.,0.,0.));
#6545=DIRECTION('center_axis',(0.,1.,0.));
#6546=DIRECTION('ref_axis',(1.,0.,0.));
#6547=DIRECTION('center_axis',(0.,1.,0.));
#6548=DIRECTION('ref_axis',(1.,0.,0.));
#6549=DIRECTION('',(0.,1.,0.));
#6550=DIRECTION('center_axis',(0.,-1.,0.));
#6551=DIRECTION('ref_axis',(1.,0.,0.));
#6552=DIRECTION('center_axis',(0.,1.,0.));
#6553=DIRECTION('ref_axis',(1.,0.,0.));
#6554=DIRECTION('center_axis',(0.,1.,0.));
#6555=DIRECTION('ref_axis',(1.,0.,0.));
#6556=DIRECTION('',(0.,1.,0.));
#6557=DIRECTION('center_axis',(0.,-1.,0.));
#6558=DIRECTION('ref_axis',(1.,0.,0.));
#6559=DIRECTION('center_axis',(0.,0.,1.));
#6560=DIRECTION('ref_axis',(1.,0.,0.));
#6561=DIRECTION('center_axis',(0.,0.,1.));
#6562=DIRECTION('ref_axis',(1.,0.,0.));
#6563=DIRECTION('',(0.,0.,1.));
#6564=DIRECTION('center_axis',(0.,0.,-1.));
#6565=DIRECTION('ref_axis',(1.,0.,0.));
#6566=DIRECTION('center_axis',(0.,0.,1.));
#6567=DIRECTION('ref_axis',(1.,0.,0.));
#6568=DIRECTION('center_axis',(0.,0.,1.));
#6569=DIRECTION('ref_axis',(1.,0.,0.));
#6570=DIRECTION('',(0.,0.,1.));
#6571=DIRECTION('center_axis',(0.,0.,-1.));
#6572=DIRECTION('ref_axis',(1.,0.,0.));
#6573=DIRECTION('center_axis',(0.,0.,1.));
#6574=DIRECTION('ref_axis',(1.,0.,0.));
#6575=DIRECTION('center_axis',(0.,0.,1.));
#6576=DIRECTION('ref_axis',(1.,0.,0.));
#6577=DIRECTION('',(0.,0.,1.));
#6578=DIRECTION('center_axis',(0.,0.,-1.));
#6579=DIRECTION('ref_axis',(1.,0.,0.));
#6580=DIRECTION('center_axis',(0.,0.,1.));
#6581=DIRECTION('ref_axis',(1.,0.,0.));
#6582=DIRECTION('center_axis',(0.,0.,1.));
#6583=DIRECTION('ref_axis',(1.,0.,0.));
#6584=DIRECTION('',(0.,0.,1.));
#6585=DIRECTION('center_axis',(0.,0.,-1.));
#6586=DIRECTION('ref_axis',(1.,0.,0.));
#6587=DIRECTION('center_axis',(0.,1.,0.));
#6588=DIRECTION('ref_axis',(1.,0.,0.));
#6589=DIRECTION('center_axis',(0.,1.,0.));
#6590=DIRECTION('ref_axis',(1.,0.,0.));
#6591=DIRECTION('',(0.,1.,0.));
#6592=DIRECTION('center_axis',(0.,-1.,0.));
#6593=DIRECTION('ref_axis',(1.,0.,0.));
#6594=DIRECTION('center_axis',(0.,0.,1.));
#6595=DIRECTION('ref_axis',(1.,0.,0.));
#6596=DIRECTION('',(0.,1.,0.));
#6597=DIRECTION('',(-1.,0.,0.));
#6598=DIRECTION('',(0.,1.,0.));
#6599=DIRECTION('',(1.,0.,0.));
#6600=DIRECTION('center_axis',(0.,0.,1.));
#6601=DIRECTION('ref_axis',(1.,0.,0.));
#6602=DIRECTION('',(0.,-1.,0.));
#6603=DIRECTION('',(1.,0.,0.));
#6604=DIRECTION('',(0.,1.,0.));
#6605=DIRECTION('',(-1.,0.,0.));
#6606=DIRECTION('center_axis',(-1.,0.,0.));
#6607=DIRECTION('ref_axis',(0.,0.,1.));
#6608=DIRECTION('',(0.,0.,-1.));
#6609=DIRECTION('',(0.,0.,1.));
#6610=DIRECTION('',(0.,1.,0.));
#6611=DIRECTION('center_axis',(1.,0.,0.));
#6612=DIRECTION('ref_axis',(0.,0.,-1.));
#6613=DIRECTION('',(0.,0.,1.));
#6614=DIRECTION('',(0.,1.,0.));
#6615=DIRECTION('',(0.,0.,-1.));
#6616=DIRECTION('center_axis',(0.,-1.,0.));
#6617=DIRECTION('ref_axis',(1.,0.,0.));
#6618=DIRECTION('',(0.,0.,1.));
#6619=DIRECTION('',(1.,0.,0.));
#6620=DIRECTION('',(0.,0.,1.));
#6621=DIRECTION('',(1.,0.,0.));
#6622=DIRECTION('center_axis',(1.,0.,0.));
#6623=DIRECTION('ref_axis',(0.,1.,0.));
#6624=DIRECTION('',(0.,0.,1.));
#6625=DIRECTION('',(0.,1.,0.));
#6626=DIRECTION('center_axis',(0.,1.,0.));
#6627=DIRECTION('ref_axis',(-1.,0.,0.));
#6628=DIRECTION('',(0.,0.,1.));
#6629=DIRECTION('',(-1.,0.,0.));
#6630=DIRECTION('',(-1.,0.,0.));
#6631=DIRECTION('center_axis',(-1.,0.,0.));
#6632=DIRECTION('ref_axis',(0.,-1.,0.));
#6633=DIRECTION('',(0.,-1.,0.));
#6634=DIRECTION('center_axis',(0.,0.,1.));
#6635=DIRECTION('ref_axis',(1.,0.,0.));
#6636=DIRECTION('center_axis',(0.,0.,1.));
#6637=DIRECTION('ref_axis',(1.,0.,0.));
#6638=DIRECTION('axis',(0.,0.,1.));
#6639=DIRECTION('refdir',(1.,0.,0.));
#6640=DIRECTION('center_axis',(0.,1.,0.));
#6641=DIRECTION('ref_axis',(1.,0.,0.));
#6642=DIRECTION('center_axis',(0.,-1.,0.));
#6643=DIRECTION('ref_axis',(1.,0.,0.));
#6644=DIRECTION('',(0.,-1.,0.));
#6645=DIRECTION('center_axis',(0.,-1.,0.));
#6646=DIRECTION('ref_axis',(1.,0.,0.));
#6647=DIRECTION('center_axis',(0.,1.,0.));
#6648=DIRECTION('ref_axis',(1.,0.,0.));
#6649=DIRECTION('center_axis',(0.,1.,0.));
#6650=DIRECTION('ref_axis',(1.,0.,0.));
#6651=DIRECTION('',(0.,-1.,0.));
#6652=DIRECTION('center_axis',(0.,1.,0.));
#6653=DIRECTION('ref_axis',(1.,0.,0.));
#6654=DIRECTION('center_axis',(0.,1.,0.));
#6655=DIRECTION('ref_axis',(1.,0.,0.));
#6656=DIRECTION('center_axis',(0.,1.,0.));
#6657=DIRECTION('ref_axis',(1.,0.,0.));
#6658=DIRECTION('axis',(0.,0.,1.));
#6659=DIRECTION('refdir',(1.,0.,0.));
#6660=DIRECTION('center_axis',(0.,1.,0.));
#6661=DIRECTION('ref_axis',(1.,0.,0.));
#6662=DIRECTION('center_axis',(0.,1.,0.));
#6663=DIRECTION('ref_axis',(1.,0.,0.));
#6664=DIRECTION('',(0.,1.,0.));
#6665=DIRECTION('center_axis',(0.,-1.,0.));
#6666=DIRECTION('ref_axis',(1.,0.,0.));
#6667=DIRECTION('center_axis',(0.,1.,0.));
#6668=DIRECTION('ref_axis',(1.,0.,0.));
#6669=DIRECTION('center_axis',(0.,1.,0.));
#6670=DIRECTION('ref_axis',(1.,0.,0.));
#6671=DIRECTION('',(0.,1.,0.));
#6672=DIRECTION('center_axis',(0.,-1.,0.));
#6673=DIRECTION('ref_axis',(1.,0.,0.));
#6674=DIRECTION('center_axis',(0.,1.,0.));
#6675=DIRECTION('ref_axis',(1.,0.,0.));
#6676=DIRECTION('center_axis',(0.,1.,0.));
#6677=DIRECTION('ref_axis',(1.,0.,0.));
#6678=DIRECTION('',(0.,1.,0.));
#6679=DIRECTION('center_axis',(0.,-1.,0.));
#6680=DIRECTION('ref_axis',(1.,0.,0.));
#6681=DIRECTION('center_axis',(0.,1.,0.));
#6682=DIRECTION('ref_axis',(1.,0.,0.));
#6683=DIRECTION('center_axis',(0.,1.,0.));
#6684=DIRECTION('ref_axis',(1.,0.,0.));
#6685=DIRECTION('',(0.,1.,0.));
#6686=DIRECTION('center_axis',(0.,-1.,0.));
#6687=DIRECTION('ref_axis',(1.,0.,0.));
#6688=DIRECTION('center_axis',(0.,1.,0.));
#6689=DIRECTION('ref_axis',(1.,0.,0.));
#6690=DIRECTION('center_axis',(0.,1.,0.));
#6691=DIRECTION('ref_axis',(1.,0.,0.));
#6692=DIRECTION('',(0.,-1.,0.));
#6693=DIRECTION('center_axis',(0.,-1.,0.));
#6694=DIRECTION('ref_axis',(1.,0.,0.));
#6695=DIRECTION('center_axis',(0.,1.,0.));
#6696=DIRECTION('ref_axis',(1.,0.,0.));
#6697=DIRECTION('center_axis',(0.,-1.,0.));
#6698=DIRECTION('ref_axis',(1.,0.,0.));
#6699=DIRECTION('center_axis',(0.,1.,0.));
#6700=DIRECTION('ref_axis',(1.,0.,0.));
#6701=DIRECTION('',(0.,-1.,0.));
#6702=DIRECTION('center_axis',(0.,-1.,0.));
#6703=DIRECTION('ref_axis',(1.,0.,0.));
#6704=DIRECTION('center_axis',(0.,1.,0.));
#6705=DIRECTION('ref_axis',(1.,0.,0.));
#6706=DIRECTION('center_axis',(0.,1.,0.));
#6707=DIRECTION('ref_axis',(1.,0.,0.));
#6708=DIRECTION('',(0.,-1.,0.));
#6709=DIRECTION('center_axis',(0.,1.,0.));
#6710=DIRECTION('ref_axis',(1.,0.,0.));
#6711=DIRECTION('center_axis',(0.,1.,0.));
#6712=DIRECTION('ref_axis',(1.,0.,0.));
#6713=DIRECTION('center_axis',(0.,1.,0.));
#6714=DIRECTION('ref_axis',(1.,0.,0.));
#6715=DIRECTION('axis',(0.,0.,1.));
#6716=DIRECTION('refdir',(1.,0.,0.));
#6717=DIRECTION('center_axis',(0.,1.,0.));
#6718=DIRECTION('ref_axis',(1.,0.,0.));
#6719=DIRECTION('center_axis',(0.,1.,0.));
#6720=DIRECTION('ref_axis',(1.,0.,0.));
#6721=DIRECTION('',(0.,1.,0.));
#6722=DIRECTION('center_axis',(0.,-1.,0.));
#6723=DIRECTION('ref_axis',(1.,0.,0.));
#6724=DIRECTION('center_axis',(0.,1.,0.));
#6725=DIRECTION('ref_axis',(1.,0.,0.));
#6726=DIRECTION('center_axis',(0.,1.,0.));
#6727=DIRECTION('ref_axis',(1.,0.,0.));
#6728=DIRECTION('',(0.,1.,0.));
#6729=DIRECTION('center_axis',(0.,-1.,0.));
#6730=DIRECTION('ref_axis',(1.,0.,0.));
#6731=DIRECTION('center_axis',(0.,1.,0.));
#6732=DIRECTION('ref_axis',(1.,0.,0.));
#6733=DIRECTION('center_axis',(0.,1.,0.));
#6734=DIRECTION('ref_axis',(1.,0.,0.));
#6735=DIRECTION('',(0.,1.,0.));
#6736=DIRECTION('center_axis',(0.,-1.,0.));
#6737=DIRECTION('ref_axis',(1.,0.,0.));
#6738=DIRECTION('center_axis',(0.,1.,0.));
#6739=DIRECTION('ref_axis',(1.,0.,0.));
#6740=DIRECTION('center_axis',(0.,1.,0.));
#6741=DIRECTION('ref_axis',(1.,0.,0.));
#6742=DIRECTION('',(0.,1.,0.));
#6743=DIRECTION('center_axis',(0.,-1.,0.));
#6744=DIRECTION('ref_axis',(1.,0.,0.));
#6745=DIRECTION('center_axis',(0.,1.,0.));
#6746=DIRECTION('ref_axis',(1.,0.,0.));
#6747=DIRECTION('center_axis',(0.,1.,0.));
#6748=DIRECTION('ref_axis',(1.,0.,0.));
#6749=DIRECTION('',(0.,-1.,0.));
#6750=DIRECTION('center_axis',(0.,1.,0.));
#6751=DIRECTION('ref_axis',(1.,0.,0.));
#6752=DIRECTION('center_axis',(0.,1.,0.));
#6753=DIRECTION('ref_axis',(1.,0.,0.));
#6754=DIRECTION('center_axis',(0.,-1.,0.));
#6755=DIRECTION('ref_axis',(1.,0.,0.));
#6756=DIRECTION('center_axis',(0.,1.,0.));
#6757=DIRECTION('ref_axis',(1.,0.,0.));
#6758=DIRECTION('center_axis',(0.,-1.,0.));
#6759=DIRECTION('ref_axis',(1.,0.,0.));
#6760=DIRECTION('',(0.,-1.,0.));
#6761=DIRECTION('center_axis',(0.,1.,0.));
#6762=DIRECTION('ref_axis',(1.,0.,0.));
#6763=DIRECTION('center_axis',(0.,1.,0.));
#6764=DIRECTION('ref_axis',(1.,0.,0.));
#6765=DIRECTION('',(0.,-1.,0.));
#6766=DIRECTION('center_axis',(0.,1.,0.));
#6767=DIRECTION('ref_axis',(1.,0.,0.));
#6768=DIRECTION('center_axis',(0.,1.,0.));
#6769=DIRECTION('ref_axis',(1.,0.,0.));
#6770=DIRECTION('center_axis',(0.,1.,0.));
#6771=DIRECTION('ref_axis',(1.,0.,0.));
#6772=DIRECTION('axis',(0.,0.,1.));
#6773=DIRECTION('refdir',(1.,0.,0.));
#6774=DIRECTION('center_axis',(0.,1.,0.));
#6775=DIRECTION('ref_axis',(1.,0.,0.));
#6776=DIRECTION('center_axis',(0.,-1.,0.));
#6777=DIRECTION('ref_axis',(1.,0.,0.));
#6778=DIRECTION('',(0.,-1.,0.));
#6779=DIRECTION('center_axis',(0.,-1.,0.));
#6780=DIRECTION('ref_axis',(1.,0.,0.));
#6781=DIRECTION('center_axis',(0.,1.,0.));
#6782=DIRECTION('ref_axis',(1.,0.,0.));
#6783=DIRECTION('center_axis',(0.,1.,0.));
#6784=DIRECTION('ref_axis',(1.,0.,0.));
#6785=DIRECTION('',(0.,-1.,0.));
#6786=DIRECTION('center_axis',(0.,1.,0.));
#6787=DIRECTION('ref_axis',(1.,0.,0.));
#6788=DIRECTION('center_axis',(0.,1.,0.));
#6789=DIRECTION('ref_axis',(1.,0.,0.));
#6790=DIRECTION('center_axis',(0.,1.,0.));
#6791=DIRECTION('ref_axis',(1.,0.,0.));
#6792=DIRECTION('axis',(0.,0.,1.));
#6793=DIRECTION('refdir',(1.,0.,0.));
#6794=DIRECTION('center_axis',(0.866025403784439,0.,-0.5));
#6795=DIRECTION('ref_axis',(0.5,0.,0.866025403784439));
#6796=DIRECTION('',(-0.5,0.,-0.866025403784439));
#6797=DIRECTION('',(0.,-1.,0.));
#6798=DIRECTION('',(0.5,0.,0.866025403784439));
#6799=DIRECTION('',(0.,-1.,0.));
#6800=DIRECTION('center_axis',(1.92296268638356E-16,0.,-1.));
#6801=DIRECTION('ref_axis',(1.,0.,1.92296268638356E-16));
#6802=DIRECTION('',(-1.,0.,-1.92296268638356E-16));
#6803=DIRECTION('',(0.,-1.,0.));
#6804=DIRECTION('',(1.,0.,1.92296268638356E-16));
#6805=DIRECTION('center_axis',(-0.866025403784439,0.,-0.5));
#6806=DIRECTION('ref_axis',(0.5,0.,-0.866025403784439));
#6807=DIRECTION('',(-0.5,0.,0.866025403784438));
#6808=DIRECTION('',(0.,-1.,0.));
#6809=DIRECTION('',(0.5,0.,-0.866025403784438));
#6810=DIRECTION('center_axis',(-0.866025403784439,0.,0.5));
#6811=DIRECTION('ref_axis',(-0.5,0.,-0.866025403784439));
#6812=DIRECTION('',(0.5,0.,0.866025403784439));
#6813=DIRECTION('',(0.,-1.,0.));
#6814=DIRECTION('',(-0.5,0.,-0.866025403784439));
#6815=DIRECTION('center_axis',(-1.92296268638356E-16,0.,1.));
#6816=DIRECTION('ref_axis',(-1.,0.,-1.92296268638356E-16));
#6817=DIRECTION('',(1.,0.,1.92296268638356E-16));
#6818=DIRECTION('',(0.,-1.,0.));
#6819=DIRECTION('',(-1.,0.,-1.92296268638356E-16));
#6820=DIRECTION('center_axis',(0.866025403784439,0.,0.5));
#6821=DIRECTION('ref_axis',(-0.5,0.,0.866025403784439));
#6822=DIRECTION('',(0.5,0.,-0.866025403784439));
#6823=DIRECTION('',(-0.5,0.,0.866025403784439));
#6824=DIRECTION('center_axis',(0.,1.,0.));
#6825=DIRECTION('ref_axis',(1.,0.,0.));
#6826=DIRECTION('center_axis',(0.,-1.,0.));
#6827=DIRECTION('ref_axis',(0.,0.,-1.));
#6828=DIRECTION('center_axis',(0.,1.,0.));
#6829=DIRECTION('ref_axis',(1.,0.,0.));
#6830=DIRECTION('center_axis',(0.,1.,0.));
#6831=DIRECTION('ref_axis',(1.,0.,0.));
#6832=DIRECTION('center_axis',(0.,1.,0.));
#6833=DIRECTION('ref_axis',(0.,0.,1.));
#6834=DIRECTION('center_axis',(0.,-1.,0.));
#6835=DIRECTION('ref_axis',(1.,0.,0.));
#6836=DIRECTION('center_axis',(0.,-1.,0.));
#6837=DIRECTION('ref_axis',(1.,0.,0.));
#6838=DIRECTION('center_axis',(0.,-1.,0.));
#6839=DIRECTION('ref_axis',(1.,0.,0.));
#6840=DIRECTION('',(0.707106781186548,0.707106781186547,8.65956056235494E-17));
#6841=DIRECTION('center_axis',(0.,-1.,0.));
#6842=DIRECTION('ref_axis',(1.,0.,0.));
#6843=DIRECTION('center_axis',(0.,-1.,0.));
#6844=DIRECTION('ref_axis',(1.,0.,0.));
#6845=DIRECTION('',(0.,1.,0.));
#6846=DIRECTION('center_axis',(0.,1.,0.));
#6847=DIRECTION('ref_axis',(1.,0.,0.));
#6848=DIRECTION('center_axis',(0.,-1.,0.));
#6849=DIRECTION('ref_axis',(1.,0.,0.));
#6850=DIRECTION('',(-0.707106781186547,0.707106781186548,-8.65956056235493E-17));
#6851=DIRECTION('center_axis',(0.,-1.,0.));
#6852=DIRECTION('ref_axis',(0.,0.,-1.));
#6853=DIRECTION('center_axis',(0.,-1.,0.));
#6854=DIRECTION('ref_axis',(1.,0.,0.));
#6855=DIRECTION('center_axis',(0.,1.,0.));
#6856=DIRECTION('ref_axis',(1.,0.,0.));
#6857=DIRECTION('center_axis',(0.,1.,0.));
#6858=DIRECTION('ref_axis',(1.,0.,0.));
#6859=DIRECTION('',(-0.447213595499958,0.894427190999916,-5.47678698264203E-17));
#6860=DIRECTION('center_axis',(0.,-1.,0.));
#6861=DIRECTION('ref_axis',(1.,0.,0.));
#6862=DIRECTION('',(0.,1.,0.));
#6863=DIRECTION('axis',(0.,0.,1.));
#6864=DIRECTION('refdir',(1.,0.,0.));
#6865=DIRECTION('axis',(0.,0.,1.));
#6866=DIRECTION('refdir',(1.,0.,0.));
#6867=DIRECTION('center_axis',(0.,-1.,0.));
#6868=DIRECTION('ref_axis',(0.,0.,-1.));
#6869=DIRECTION('center_axis',(0.,-1.,0.));
#6870=DIRECTION('ref_axis',(1.,0.,0.));
#6871=DIRECTION('center_axis',(0.,-1.,0.));
#6872=DIRECTION('ref_axis',(1.,0.,0.));
#6873=DIRECTION('center_axis',(1.,0.,1.22464679914735E-16));
#6874=DIRECTION('ref_axis',(-1.22464679914735E-16,0.,1.));
#6875=DIRECTION('center_axis',(0.,1.,0.));
#6876=DIRECTION('ref_axis',(1.,0.,0.));
#6877=DIRECTION('center_axis',(0.,1.,0.));
#6878=DIRECTION('ref_axis',(1.,0.,0.));
#6879=DIRECTION('center_axis',(0.,-1.,0.));
#6880=DIRECTION('ref_axis',(1.,0.,0.));
#6881=DIRECTION('',(0.,1.,0.));
#6882=DIRECTION('center_axis',(0.,-1.,0.));
#6883=DIRECTION('ref_axis',(1.,0.,0.));
#6884=DIRECTION('center_axis',(0.,-1.,0.));
#6885=DIRECTION('ref_axis',(1.,0.,0.));
#6886=DIRECTION('center_axis',(0.,-1.,0.));
#6887=DIRECTION('ref_axis',(1.,0.,0.));
#6888=DIRECTION('',(0.,1.,0.));
#6889=DIRECTION('center_axis',(0.,-1.,0.));
#6890=DIRECTION('ref_axis',(1.,0.,0.));
#6891=DIRECTION('center_axis',(0.,1.,0.));
#6892=DIRECTION('ref_axis',(1.,0.,0.));
#6893=DIRECTION('',(-0.707106781186548,0.707106781186547,-8.65956056235493E-17));
#6894=DIRECTION('center_axis',(0.,-1.,0.));
#6895=DIRECTION('ref_axis',(1.,0.,0.));
#6896=DIRECTION('center_axis',(0.,1.,0.));
#6897=DIRECTION('ref_axis',(0.,0.,1.));
#6898=DIRECTION('center_axis',(0.,-1.,0.));
#6899=DIRECTION('ref_axis',(1.,0.,0.));
#6900=DIRECTION('center_axis',(0.,-1.,0.));
#6901=DIRECTION('ref_axis',(1.,0.,0.));
#6902=DIRECTION('',(0.,1.,0.));
#6903=DIRECTION('center_axis',(0.,-1.,0.));
#6904=DIRECTION('ref_axis',(0.,0.,-1.));
#6905=DIRECTION('center_axis',(0.,-1.,0.));
#6906=DIRECTION('ref_axis',(1.,0.,0.));
#6907=DIRECTION('center_axis',(0.,-1.,0.));
#6908=DIRECTION('ref_axis',(1.,0.,0.));
#6909=DIRECTION('',(0.707106781186548,0.707106781186547,8.65956056235493E-17));
#6910=DIRECTION('axis',(0.,0.,1.));
#6911=DIRECTION('refdir',(1.,0.,0.));
#6912=DIRECTION('center_axis',(0.,-1.,0.));
#6913=DIRECTION('ref_axis',(0.,0.,-1.));
#6914=DIRECTION('center_axis',(0.,-1.,0.));
#6915=DIRECTION('ref_axis',(1.,0.,0.));
#6916=DIRECTION('center_axis',(0.,-1.,0.));
#6917=DIRECTION('ref_axis',(1.,0.,0.));
#6918=DIRECTION('center_axis',(1.,0.,1.22464679914735E-16));
#6919=DIRECTION('ref_axis',(-1.22464679914735E-16,0.,1.));
#6920=DIRECTION('center_axis',(0.,1.,0.));
#6921=DIRECTION('ref_axis',(1.,0.,0.));
#6922=DIRECTION('center_axis',(0.,1.,0.));
#6923=DIRECTION('ref_axis',(1.,0.,0.));
#6924=DIRECTION('center_axis',(0.,-1.,0.));
#6925=DIRECTION('ref_axis',(1.,0.,0.));
#6926=DIRECTION('center_axis',(0.,-1.,0.));
#6927=DIRECTION('ref_axis',(1.,0.,0.));
#6928=DIRECTION('',(0.,1.,0.));
#6929=DIRECTION('center_axis',(0.,1.,0.));
#6930=DIRECTION('ref_axis',(0.,0.,1.));
#6931=DIRECTION('center_axis',(0.,-1.,0.));
#6932=DIRECTION('ref_axis',(1.,0.,0.));
#6933=DIRECTION('center_axis',(0.,-1.,0.));
#6934=DIRECTION('ref_axis',(1.,0.,0.));
#6935=DIRECTION('center_axis',(0.,-1.,0.));
#6936=DIRECTION('ref_axis',(1.,0.,0.));
#6937=DIRECTION('center_axis',(0.,-1.,0.));
#6938=DIRECTION('ref_axis',(1.,0.,0.));
#6939=DIRECTION('',(0.707106781186548,0.707106781186547,8.65956056235494E-17));
#6940=DIRECTION('center_axis',(0.,-1.,0.));
#6941=DIRECTION('ref_axis',(1.,0.,0.));
#6942=DIRECTION('center_axis',(0.,-1.,0.));
#6943=DIRECTION('ref_axis',(1.,0.,0.));
#6944=DIRECTION('',(0.,1.,0.));
#6945=DIRECTION('center_axis',(0.,1.,0.));
#6946=DIRECTION('ref_axis',(1.,0.,0.));
#6947=DIRECTION('center_axis',(0.,-1.,0.));
#6948=DIRECTION('ref_axis',(1.,0.,0.));
#6949=DIRECTION('',(-0.707106781186548,0.707106781186547,-8.65956056235494E-17));
#6950=DIRECTION('center_axis',(0.,-1.,0.));
#6951=DIRECTION('ref_axis',(0.,0.,-1.));
#6952=DIRECTION('center_axis',(0.,-1.,0.));
#6953=DIRECTION('ref_axis',(1.,0.,0.));
#6954=DIRECTION('',(0.,1.,0.));
#6955=DIRECTION('axis',(0.,0.,1.));
#6956=DIRECTION('refdir',(1.,0.,0.));
#6957=DIRECTION('center_axis',(0.,0.,1.));
#6958=DIRECTION('ref_axis',(1.,0.,0.));
#6959=DIRECTION('center_axis',(1.22464679914735E-16,-1.,0.));
#6960=DIRECTION('ref_axis',(-1.,-1.22464679914735E-16,0.));
#6961=DIRECTION('center_axis',(0.78183148246803,0.,0.623489801858733));
#6962=DIRECTION('ref_axis',(0.623489801858734,0.,-0.78183148246803));
#6963=DIRECTION('center_axis',(7.63554790147315E-17,-1.,-9.57467422477103E-17));
#6964=DIRECTION('ref_axis',(-0.623489801858734,-1.22464679914735E-16,0.78183148246803));
#6965=DIRECTION('center_axis',(0.974927912181824,0.,-0.222520933956314));
#6966=DIRECTION('ref_axis',(-0.222520933956314,0.,-0.974927912181824));
#6967=DIRECTION('center_axis',(-2.7250954951288E-17,-1.,-1.19394234705288E-16));
#6968=DIRECTION('ref_axis',(0.222520933956314,-1.22464679914735E-16,0.974927912181824));
#6969=DIRECTION('center_axis',(0.433883739117558,0.,-0.900968867902419));
#6970=DIRECTION('ref_axis',(-0.900968867902419,0.,-0.433883739117558));
#6971=DIRECTION('center_axis',(-1.10336864020811E-16,-1.,-5.31354332312403E-17));
#6972=DIRECTION('ref_axis',(0.900968867902419,-1.22464679914735E-16,0.433883739117558));
#6973=DIRECTION('center_axis',(-0.433883739117558,0.,-0.900968867902419));
#6974=DIRECTION('ref_axis',(-0.900968867902419,0.,0.433883739117558));
#6975=DIRECTION('center_axis',(-1.10336864020811E-16,-1.,5.31354332312403E-17));
#6976=DIRECTION('ref_axis',(0.900968867902419,-1.22464679914735E-16,-0.433883739117558));
#6977=DIRECTION('center_axis',(-0.974927912181824,0.,-0.222520933956314));
#6978=DIRECTION('ref_axis',(-0.222520933956315,0.,0.974927912181824));
#6979=DIRECTION('center_axis',(-2.7250954951288E-17,-1.,1.19394234705288E-16));
#6980=DIRECTION('ref_axis',(0.222520933956315,-1.22464679914735E-16,-0.974927912181824));
#6981=DIRECTION('center_axis',(-0.78183148246803,0.,0.623489801858734));
#6982=DIRECTION('ref_axis',(0.623489801858733,0.,0.78183148246803));
#6983=DIRECTION('center_axis',(7.63554790147315E-17,-1.,9.57467422477103E-17));
#6984=DIRECTION('ref_axis',(-0.623489801858733,-1.22464679914735E-16,-0.78183148246803));
#6985=DIRECTION('axis',(0.,0.,1.));
#6986=DIRECTION('refdir',(1.,0.,0.));
#6987=DIRECTION('center_axis',(0.,0.,1.));
#6988=DIRECTION('ref_axis',(1.,0.,0.));
#6989=DIRECTION('center_axis',(0.,-1.,0.));
#6990=DIRECTION('ref_axis',(0.,0.,-1.));
#6991=DIRECTION('center_axis',(0.,-1.,0.));
#6992=DIRECTION('ref_axis',(0.,0.,-1.));
#6993=DIRECTION('center_axis',(0.,1.,0.));
#6994=DIRECTION('ref_axis',(1.,0.,0.));
#6995=DIRECTION('center_axis',(0.,1.,0.));
#6996=DIRECTION('ref_axis',(1.,0.,0.));
#6997=DIRECTION('center_axis',(0.,1.,0.));
#6998=DIRECTION('ref_axis',(1.,0.,0.));
#6999=DIRECTION('center_axis',(0.,1.,0.));
#7000=DIRECTION('ref_axis',(1.,0.,0.));
#7001=DIRECTION('',(0.,-1.,0.));
#7002=DIRECTION('center_axis',(0.,-1.,0.));
#7003=DIRECTION('ref_axis',(1.,0.,0.));
#7004=DIRECTION('center_axis',(0.,1.,0.));
#7005=DIRECTION('ref_axis',(1.,0.,0.));
#7006=DIRECTION('center_axis',(0.,1.,0.));
#7007=DIRECTION('ref_axis',(1.,0.,0.));
#7008=DIRECTION('center_axis',(0.,1.,0.));
#7009=DIRECTION('ref_axis',(1.,0.,0.));
#7010=DIRECTION('center_axis',(0.,1.,0.));
#7011=DIRECTION('ref_axis',(1.,0.,0.));
#7012=DIRECTION('center_axis',(0.,1.,0.));
#7013=DIRECTION('ref_axis',(1.,0.,0.));
#7014=DIRECTION('center_axis',(0.,1.,0.));
#7015=DIRECTION('ref_axis',(1.,0.,0.));
#7016=DIRECTION('center_axis',(0.,-1.,0.));
#7017=DIRECTION('ref_axis',(1.,0.,0.));
#7018=DIRECTION('center_axis',(0.,-1.,0.));
#7019=DIRECTION('ref_axis',(0.,0.,-1.));
#7020=DIRECTION('center_axis',(8.96625347776458E-17,0.,1.));
#7021=DIRECTION('ref_axis',(1.,0.,0.));
#7022=DIRECTION('center_axis',(0.,-1.,0.));
#7023=DIRECTION('ref_axis',(0.,0.,-1.));
#7024=DIRECTION('center_axis',(0.,1.,0.));
#7025=DIRECTION('ref_axis',(1.,0.,0.));
#7026=DIRECTION('center_axis',(0.,-1.,0.));
#7027=DIRECTION('ref_axis',(1.,0.,0.));
#7028=DIRECTION('center_axis',(0.,-1.,0.));
#7029=DIRECTION('ref_axis',(0.,0.,-1.));
#7030=DIRECTION('center_axis',(0.,0.,1.));
#7031=DIRECTION('ref_axis',(1.,0.,0.));
#7032=DIRECTION('center_axis',(0.,-1.,0.));
#7033=DIRECTION('ref_axis',(0.,0.,-1.));
#7034=DIRECTION('center_axis',(0.,1.,0.));
#7035=DIRECTION('ref_axis',(1.,0.,0.));
#7036=DIRECTION('center_axis',(0.,-1.,0.));
#7037=DIRECTION('ref_axis',(1.,0.,0.));
#7038=DIRECTION('center_axis',(0.,-1.,0.));
#7039=DIRECTION('ref_axis',(1.,0.,0.));
#7040=DIRECTION('center_axis',(0.,-1.,0.));
#7041=DIRECTION('ref_axis',(0.,0.,-1.));
#7042=DIRECTION('center_axis',(0.,0.,1.));
#7043=DIRECTION('ref_axis',(1.,0.,0.));
#7044=DIRECTION('center_axis',(0.,-1.,0.));
#7045=DIRECTION('ref_axis',(0.,0.,-1.));
#7046=DIRECTION('center_axis',(0.,1.,0.));
#7047=DIRECTION('ref_axis',(1.,0.,0.));
#7048=DIRECTION('center_axis',(0.,-1.,0.));
#7049=DIRECTION('ref_axis',(1.,0.,0.));
#7050=DIRECTION('center_axis',(0.,-1.,0.));
#7051=DIRECTION('ref_axis',(0.,0.,-1.));
#7052=DIRECTION('center_axis',(8.96625347776458E-17,0.,1.));
#7053=DIRECTION('ref_axis',(1.,0.,0.));
#7054=DIRECTION('center_axis',(0.,-1.,0.));
#7055=DIRECTION('ref_axis',(0.,0.,-1.));
#7056=DIRECTION('center_axis',(0.,1.,0.));
#7057=DIRECTION('ref_axis',(1.,0.,0.));
#7058=DIRECTION('center_axis',(0.,-1.,0.));
#7059=DIRECTION('ref_axis',(1.,0.,0.));
#7060=DIRECTION('center_axis',(0.,-1.,0.));
#7061=DIRECTION('ref_axis',(0.,0.,-1.));
#7062=DIRECTION('center_axis',(0.,0.,1.));
#7063=DIRECTION('ref_axis',(1.,0.,0.));
#7064=DIRECTION('center_axis',(0.,-1.,0.));
#7065=DIRECTION('ref_axis',(0.,0.,-1.));
#7066=DIRECTION('center_axis',(0.,1.,0.));
#7067=DIRECTION('ref_axis',(1.,0.,0.));
#7068=DIRECTION('center_axis',(0.,1.,0.));
#7069=DIRECTION('ref_axis',(1.,0.,0.));
#7070=DIRECTION('',(0.,1.,0.));
#7071=DIRECTION('center_axis',(0.,-1.,0.));
#7072=DIRECTION('ref_axis',(1.,0.,0.));
#7073=DIRECTION('center_axis',(0.,-1.,0.));
#7074=DIRECTION('ref_axis',(1.,0.,0.));
#7075=DIRECTION('center_axis',(0.,1.,0.));
#7076=DIRECTION('ref_axis',(1.,0.,0.));
#7077=DIRECTION('center_axis',(0.,-1.,0.));
#7078=DIRECTION('ref_axis',(0.,0.,-1.));
#7079=DIRECTION('center_axis',(0.,0.,1.));
#7080=DIRECTION('ref_axis',(1.,0.,0.));
#7081=DIRECTION('center_axis',(0.,-1.,0.));
#7082=DIRECTION('ref_axis',(0.,0.,-1.));
#7083=DIRECTION('center_axis',(0.,-1.,0.));
#7084=DIRECTION('ref_axis',(-1.,0.,0.));
#7085=DIRECTION('center_axis',(0.,1.,0.));
#7086=DIRECTION('ref_axis',(1.,0.,0.));
#7087=DIRECTION('axis',(0.,0.,1.));
#7088=DIRECTION('refdir',(1.,0.,0.));
#7089=DIRECTION('center_axis',(0.,1.,0.));
#7090=DIRECTION('ref_axis',(0.,0.,1.));
#7091=DIRECTION('center_axis',(0.,-1.,0.));
#7092=DIRECTION('ref_axis',(1.,0.,0.));
#7093=DIRECTION('center_axis',(0.,-1.,0.));
#7094=DIRECTION('ref_axis',(1.,0.,0.));
#7095=DIRECTION('center_axis',(0.,-1.,0.));
#7096=DIRECTION('ref_axis',(1.,0.,0.));
#7097=DIRECTION('center_axis',(0.,-1.,0.));
#7098=DIRECTION('ref_axis',(1.,0.,0.));
#7099=DIRECTION('',(0.,1.,0.));
#7100=DIRECTION('center_axis',(0.,-1.,0.));
#7101=DIRECTION('ref_axis',(0.,0.,-1.));
#7102=DIRECTION('center_axis',(0.,-1.,0.));
#7103=DIRECTION('ref_axis',(1.,0.,0.));
#7104=DIRECTION('center_axis',(0.,-1.,0.));
#7105=DIRECTION('ref_axis',(1.,0.,0.));
#7106=DIRECTION('',(0.,1.,0.));
#7107=DIRECTION('center_axis',(0.,1.,0.));
#7108=DIRECTION('ref_axis',(0.,0.,1.));
#7109=DIRECTION('center_axis',(0.,-1.,0.));
#7110=DIRECTION('ref_axis',(1.,0.,0.));
#7111=DIRECTION('center_axis',(0.,-1.,0.));
#7112=DIRECTION('ref_axis',(1.,0.,0.));
#7113=DIRECTION('center_axis',(0.,-1.,0.));
#7114=DIRECTION('ref_axis',(1.,0.,0.));
#7115=DIRECTION('center_axis',(0.,-1.,0.));
#7116=DIRECTION('ref_axis',(1.,0.,0.));
#7117=DIRECTION('',(0.,1.,0.));
#7118=DIRECTION('center_axis',(0.,-1.,0.));
#7119=DIRECTION('ref_axis',(0.,0.,-1.));
#7120=DIRECTION('center_axis',(0.,-1.,0.));
#7121=DIRECTION('ref_axis',(1.,0.,0.));
#7122=DIRECTION('center_axis',(0.,-1.,0.));
#7123=DIRECTION('ref_axis',(1.,0.,0.));
#7124=DIRECTION('',(0.,1.,0.));
#7125=DIRECTION('',(0.,0.,1.));
#7126=DIRECTION('',(1.,0.,0.));
#7127=DIRECTION('',(0.,0.,1.));
#7128=DIRECTION('',(1.,0.,0.));
#7129=DIRECTION('',(0.,0.,1.));
#7130=DIRECTION('',(1.,0.,0.));
#7131=DIRECTION('',(0.,0.,1.));
#7132=DIRECTION('',(1.,0.,0.));
#7133=DIRECTION('',(0.,0.,1.));
#7134=DIRECTION('',(1.,0.,0.));
#7135=DIRECTION('axis',(0.,0.,1.));
#7136=DIRECTION('refdir',(1.,0.,0.));
#7137=DIRECTION('axis',(0.,0.,1.));
#7138=DIRECTION('refdir',(1.,0.,0.));
#7139=DIRECTION('center_axis',(-1.,0.,0.));
#7140=DIRECTION('ref_axis',(0.,0.,1.));
#7141=DIRECTION('',(0.,-1.,0.));
#7142=DIRECTION('',(0.,0.,1.));
#7143=DIRECTION('',(0.,1.,0.));
#7144=DIRECTION('',(0.,0.,-1.));
#7145=DIRECTION('center_axis',(0.,1.,0.));
#7146=DIRECTION('ref_axis',(1.,0.,0.));
#7147=DIRECTION('center_axis',(0.,-1.,0.));
#7148=DIRECTION('ref_axis',(1.,0.,0.));
#7149=DIRECTION('',(-1.,0.,0.));
#7150=DIRECTION('',(0.,0.,1.));
#7151=DIRECTION('center_axis',(1.,0.,0.));
#7152=DIRECTION('ref_axis',(0.,0.,-1.));
#7153=DIRECTION('',(0.,1.,0.));
#7154=DIRECTION('',(0.,1.,0.));
#7155=DIRECTION('',(0.,0.,-1.));
#7156=DIRECTION('center_axis',(0.,0.,1.));
#7157=DIRECTION('ref_axis',(1.,0.,0.));
#7158=DIRECTION('',(1.,0.,0.));
#7159=DIRECTION('center_axis',(0.,1.,0.));
#7160=DIRECTION('ref_axis',(0.,0.,1.));
#7161=DIRECTION('center_axis',(0.,1.,0.));
#7162=DIRECTION('ref_axis',(1.,0.,0.));
#7163=DIRECTION('center_axis',(0.,1.,0.));
#7164=DIRECTION('ref_axis',(1.,0.,0.));
#7165=DIRECTION('center_axis',(0.,1.,0.));
#7166=DIRECTION('ref_axis',(1.,0.,0.));
#7167=DIRECTION('center_axis',(0.,1.,0.));
#7168=DIRECTION('ref_axis',(1.,0.,0.));
#7169=DIRECTION('center_axis',(0.,1.,0.));
#7170=DIRECTION('ref_axis',(1.,0.,0.));
#7171=DIRECTION('center_axis',(0.,1.,0.));
#7172=DIRECTION('ref_axis',(1.,0.,0.));
#7173=DIRECTION('center_axis',(0.,-1.,0.));
#7174=DIRECTION('ref_axis',(1.,0.,0.));
#7175=DIRECTION('center_axis',(0.,1.,0.));
#7176=DIRECTION('ref_axis',(1.,0.,0.));
#7177=DIRECTION('',(0.,-1.,0.));
#7178=DIRECTION('center_axis',(0.,1.,0.));
#7179=DIRECTION('ref_axis',(1.,0.,0.));
#7180=DIRECTION('',(0.,-1.,0.));
#7181=DIRECTION('center_axis',(0.,1.,0.));
#7182=DIRECTION('ref_axis',(1.,0.,0.));
#7183=DIRECTION('center_axis',(0.,1.,0.));
#7184=DIRECTION('ref_axis',(1.,0.,0.));
#7185=DIRECTION('center_axis',(0.,1.,0.));
#7186=DIRECTION('ref_axis',(1.,0.,0.));
#7187=DIRECTION('',(0.,-1.,0.));
#7188=DIRECTION('center_axis',(0.,1.,0.));
#7189=DIRECTION('ref_axis',(1.,0.,0.));
#7190=DIRECTION('center_axis',(0.,1.,0.));
#7191=DIRECTION('ref_axis',(1.,0.,0.));
#7192=DIRECTION('axis',(0.,0.,1.));
#7193=DIRECTION('refdir',(1.,0.,0.));
#7194=DIRECTION('center_axis',(0.,1.,0.));
#7195=DIRECTION('ref_axis',(1.,0.,0.));
#7196=DIRECTION('center_axis',(0.,1.,0.));
#7197=DIRECTION('ref_axis',(1.,0.,0.));
#7198=DIRECTION('',(0.,1.,0.));
#7199=DIRECTION('center_axis',(0.,-1.,0.));
#7200=DIRECTION('ref_axis',(1.,0.,0.));
#7201=DIRECTION('center_axis',(0.,1.,0.));
#7202=DIRECTION('ref_axis',(1.,0.,0.));
#7203=DIRECTION('center_axis',(0.,1.,0.));
#7204=DIRECTION('ref_axis',(1.,0.,0.));
#7205=DIRECTION('',(0.,1.,0.));
#7206=DIRECTION('center_axis',(0.,-1.,0.));
#7207=DIRECTION('ref_axis',(1.,0.,0.));
#7208=DIRECTION('center_axis',(0.,0.,1.));
#7209=DIRECTION('ref_axis',(1.,0.,0.));
#7210=DIRECTION('',(0.,1.,0.));
#7211=DIRECTION('center_axis',(0.,0.,1.));
#7212=DIRECTION('ref_axis',(1.,0.,0.));
#7213=DIRECTION('center_axis',(0.,0.,1.));
#7214=DIRECTION('ref_axis',(1.,0.,0.));
#7215=DIRECTION('center_axis',(0.,0.,1.));
#7216=DIRECTION('ref_axis',(1.,0.,0.));
#7217=DIRECTION('',(0.,0.,1.));
#7218=DIRECTION('center_axis',(0.,0.,1.));
#7219=DIRECTION('ref_axis',(1.,0.,0.));
#7220=DIRECTION('center_axis',(0.,0.,1.));
#7221=DIRECTION('ref_axis',(1.,0.,0.));
#7222=DIRECTION('',(0.,-1.,0.));
#7223=DIRECTION('center_axis',(-1.,0.,0.));
#7224=DIRECTION('ref_axis',(0.,0.,1.));
#7225=DIRECTION('',(0.,0.,1.));
#7226=DIRECTION('',(0.,1.,0.));
#7227=DIRECTION('',(0.,0.,-1.));
#7228=DIRECTION('',(0.,1.,0.));
#7229=DIRECTION('center_axis',(0.,0.,-1.));
#7230=DIRECTION('ref_axis',(-1.,0.,0.));
#7231=DIRECTION('',(-1.,0.,0.));
#7232=DIRECTION('',(0.,1.,0.));
#7233=DIRECTION('',(1.,0.,0.));
#7234=DIRECTION('center_axis',(1.,0.,0.));
#7235=DIRECTION('ref_axis',(0.,0.,-1.));
#7236=DIRECTION('',(0.,0.,-1.));
#7237=DIRECTION('',(0.,-1.,0.));
#7238=DIRECTION('',(0.,0.,1.));
#7239=DIRECTION('center_axis',(0.,1.,0.));
#7240=DIRECTION('ref_axis',(1.,0.,0.));
#7241=DIRECTION('center_axis',(0.,1.,0.));
#7242=DIRECTION('ref_axis',(1.,0.,0.));
#7243=DIRECTION('center_axis',(0.,-1.,0.));
#7244=DIRECTION('ref_axis',(1.,0.,0.));
#7245=DIRECTION('center_axis',(0.,1.,0.));
#7246=DIRECTION('ref_axis',(-1.83697019872103E-16,0.,1.));
#7247=DIRECTION('center_axis',(0.,-1.,0.));
#7248=DIRECTION('ref_axis',(1.,0.,0.));
#7249=DIRECTION('center_axis',(0.866025403784438,0.,-0.5));
#7250=DIRECTION('ref_axis',(-0.5,0.,-0.866025403784438));
#7251=DIRECTION('',(0.,-1.,0.));
#7252=DIRECTION('',(-0.5,0.,-0.866025403784438));
#7253=DIRECTION('',(0.,1.,0.));
#7254=DIRECTION('',(0.5,0.,0.866025403784438));
#7255=DIRECTION('center_axis',(-0.866025403784438,0.,0.5));
#7256=DIRECTION('ref_axis',(0.5,0.,0.866025403784438));
#7257=DIRECTION('',(0.,1.,0.));
#7258=DIRECTION('',(-0.5,0.,-0.866025403784438));
#7259=DIRECTION('',(0.,-1.,0.));
#7260=DIRECTION('',(0.5,0.,0.866025403784438));
#7261=DIRECTION('center_axis',(0.,1.,0.));
#7262=DIRECTION('ref_axis',(1.,0.,0.));
#7263=DIRECTION('center_axis',(0.,1.,0.));
#7264=DIRECTION('ref_axis',(1.,0.,0.));
#7265=DIRECTION('center_axis',(0.,-1.,0.));
#7266=DIRECTION('ref_axis',(1.,0.,0.));
#7267=DIRECTION('',(0.5,0.,-0.866025403784439));
#7268=DIRECTION('center_axis',(0.,-1.,0.));
#7269=DIRECTION('ref_axis',(1.,0.,0.));
#7270=DIRECTION('',(-0.5,0.,0.866025403784439));
#7271=DIRECTION('center_axis',(0.,-1.,0.));
#7272=DIRECTION('ref_axis',(1.,0.,0.));
#7273=DIRECTION('',(-1.,0.,0.));
#7274=DIRECTION('center_axis',(0.,-1.,0.));
#7275=DIRECTION('ref_axis',(1.,0.,0.));
#7276=DIRECTION('',(1.,0.,0.));
#7277=DIRECTION('center_axis',(0.,-1.,0.));
#7278=DIRECTION('ref_axis',(1.,0.,0.));
#7279=DIRECTION('center_axis',(0.,-1.,0.));
#7280=DIRECTION('ref_axis',(1.,0.,0.));
#7281=DIRECTION('center_axis',(0.,1.,0.));
#7282=DIRECTION('ref_axis',(-1.,0.,3.21624529935327E-16));
#7283=DIRECTION('center_axis',(0.,-1.,0.));
#7284=DIRECTION('ref_axis',(1.,0.,0.));
#7285=DIRECTION('',(0.,-1.,0.));
#7286=DIRECTION('center_axis',(-0.866025403784439,0.,-0.5));
#7287=DIRECTION('ref_axis',(-0.5,0.,0.866025403784439));
#7288=DIRECTION('',(-0.5,0.,0.866025403784439));
#7289=DIRECTION('',(0.,1.,0.));
#7290=DIRECTION('center_axis',(0.866025403784439,0.,0.5));
#7291=DIRECTION('ref_axis',(0.5,0.,-0.866025403784439));
#7292=DIRECTION('',(0.,1.,0.));
#7293=DIRECTION('',(0.,-1.,0.));
#7294=DIRECTION('',(0.5,0.,-0.866025403784439));
#7295=DIRECTION('center_axis',(0.,1.,0.));
#7296=DIRECTION('ref_axis',(1.,0.,0.));
#7297=DIRECTION('center_axis',(0.,-1.,0.));
#7298=DIRECTION('ref_axis',(1.,0.,0.));
#7299=DIRECTION('',(0.,-1.,0.));
#7300=DIRECTION('center_axis',(0.,0.,1.));
#7301=DIRECTION('ref_axis',(1.,0.,0.));
#7302=DIRECTION('',(0.,1.,0.));
#7303=DIRECTION('',(1.,0.,0.));
#7304=DIRECTION('center_axis',(0.,0.,-1.));
#7305=DIRECTION('ref_axis',(-1.,0.,0.));
#7306=DIRECTION('',(0.,-1.,0.));
#7307=DIRECTION('',(-1.,0.,0.));
#7308=DIRECTION('',(0.,1.,0.));
#7309=DIRECTION('center_axis',(0.,1.,0.));
#7310=DIRECTION('ref_axis',(1.,0.,0.));
#7311=DIRECTION('center_axis',(0.,1.,0.));
#7312=DIRECTION('ref_axis',(1.,0.,0.));
#7313=DIRECTION('center_axis',(0.,-1.,0.));
#7314=DIRECTION('ref_axis',(1.,0.,0.));
#7315=DIRECTION('center_axis',(0.,1.,0.));
#7316=DIRECTION('ref_axis',(1.,0.,0.));
#7317=DIRECTION('center_axis',(0.,1.,0.));
#7318=DIRECTION('ref_axis',(1.,0.,0.));
#7319=DIRECTION('center_axis',(0.,1.,0.));
#7320=DIRECTION('ref_axis',(1.,0.,0.));
#7321=DIRECTION('center_axis',(0.,1.,0.));
#7322=DIRECTION('ref_axis',(1.,0.,0.));
#7323=DIRECTION('center_axis',(0.,1.,0.));
#7324=DIRECTION('ref_axis',(1.,0.,0.));
#7325=DIRECTION('',(0.,-1.,0.));
#7326=DIRECTION('center_axis',(0.,1.,0.));
#7327=DIRECTION('ref_axis',(1.,0.,0.));
#7328=DIRECTION('',(0.,-1.,0.));
#7329=DIRECTION('center_axis',(0.,1.,0.));
#7330=DIRECTION('ref_axis',(1.,0.,0.));
#7331=DIRECTION('center_axis',(0.,1.,0.));
#7332=DIRECTION('ref_axis',(1.,0.,0.));
#7333=DIRECTION('axis',(0.,0.,1.));
#7334=DIRECTION('refdir',(1.,0.,0.));
#7335=DIRECTION('center_axis',(0.,1.,0.));
#7336=DIRECTION('ref_axis',(1.,0.,0.));
#7337=DIRECTION('center_axis',(0.,-1.,0.));
#7338=DIRECTION('ref_axis',(1.,0.,0.));
#7339=DIRECTION('',(0.,-1.,0.));
#7340=DIRECTION('center_axis',(0.,-1.,0.));
#7341=DIRECTION('ref_axis',(1.,0.,0.));
#7342=DIRECTION('center_axis',(0.,1.,0.));
#7343=DIRECTION('ref_axis',(1.,0.,0.));
#7344=DIRECTION('center_axis',(0.,1.,0.));
#7345=DIRECTION('ref_axis',(1.,0.,0.));
#7346=DIRECTION('',(0.,-1.,0.));
#7347=DIRECTION('center_axis',(0.,1.,0.));
#7348=DIRECTION('ref_axis',(1.,0.,0.));
#7349=DIRECTION('center_axis',(0.,1.,0.));
#7350=DIRECTION('ref_axis',(1.,0.,0.));
#7351=DIRECTION('center_axis',(0.,1.,0.));
#7352=DIRECTION('ref_axis',(1.,0.,0.));
#7353=DIRECTION('axis',(0.,0.,1.));
#7354=DIRECTION('refdir',(1.,0.,0.));
#7355=DIRECTION('center_axis',(0.,0.,1.));
#7356=DIRECTION('ref_axis',(1.,0.,0.));
#7357=DIRECTION('',(0.,1.,0.));
#7358=DIRECTION('center_axis',(0.,0.,1.));
#7359=DIRECTION('ref_axis',(1.,0.,0.));
#7360=DIRECTION('center_axis',(0.,0.,1.));
#7361=DIRECTION('ref_axis',(1.,0.,0.));
#7362=DIRECTION('center_axis',(0.,0.,1.));
#7363=DIRECTION('ref_axis',(1.,0.,0.));
#7364=DIRECTION('',(0.,0.,1.));
#7365=DIRECTION('center_axis',(0.,0.,1.));
#7366=DIRECTION('ref_axis',(1.,0.,0.));
#7367=DIRECTION('center_axis',(0.,0.,1.));
#7368=DIRECTION('ref_axis',(1.,0.,0.));
#7369=DIRECTION('',(0.,-1.,0.));
#7370=DIRECTION('center_axis',(0.,1.,0.));
#7371=DIRECTION('ref_axis',(1.,0.,0.));
#7372=DIRECTION('center_axis',(0.,-1.,0.));
#7373=DIRECTION('ref_axis',(1.,0.,0.));
#7374=DIRECTION('',(0.,-1.,0.));
#7375=DIRECTION('center_axis',(0.,-1.,0.));
#7376=DIRECTION('ref_axis',(1.,0.,0.));
#7377=DIRECTION('center_axis',(0.,1.,0.));
#7378=DIRECTION('ref_axis',(1.,0.,0.));
#7379=DIRECTION('center_axis',(0.,1.,0.));
#7380=DIRECTION('ref_axis',(1.,0.,0.));
#7381=DIRECTION('',(0.,-1.,0.));
#7382=DIRECTION('center_axis',(0.,1.,0.));
#7383=DIRECTION('ref_axis',(1.,0.,0.));
#7384=DIRECTION('center_axis',(0.,1.,0.));
#7385=DIRECTION('ref_axis',(1.,0.,0.));
#7386=DIRECTION('center_axis',(0.,1.,0.));
#7387=DIRECTION('ref_axis',(1.,0.,0.));
#7388=DIRECTION('axis',(0.,0.,1.));
#7389=DIRECTION('refdir',(1.,0.,0.));
#7390=DIRECTION('center_axis',(0.,1.,0.));
#7391=DIRECTION('ref_axis',(1.,0.,0.));
#7392=DIRECTION('center_axis',(0.,1.,0.));
#7393=DIRECTION('ref_axis',(1.,0.,0.));
#7394=DIRECTION('',(0.,1.,0.));
#7395=DIRECTION('center_axis',(0.,1.,0.));
#7396=DIRECTION('ref_axis',(1.,0.,0.));
#7397=DIRECTION('center_axis',(0.,1.,0.));
#7398=DIRECTION('ref_axis',(1.,0.,0.));
#7399=DIRECTION('center_axis',(0.,1.,0.));
#7400=DIRECTION('ref_axis',(1.,0.,0.));
#7401=DIRECTION('center_axis',(0.,1.,0.));
#7402=DIRECTION('ref_axis',(1.,0.,0.));
#7403=DIRECTION('',(0.,1.,0.));
#7404=DIRECTION('center_axis',(0.,-1.,0.));
#7405=DIRECTION('ref_axis',(1.,0.,0.));
#7406=DIRECTION('center_axis',(0.,1.,0.));
#7407=DIRECTION('ref_axis',(1.,0.,0.));
#7408=DIRECTION('center_axis',(0.,1.,0.));
#7409=DIRECTION('ref_axis',(1.,0.,0.));
#7410=DIRECTION('',(0.,1.,0.));
#7411=DIRECTION('center_axis',(0.,-1.,0.));
#7412=DIRECTION('ref_axis',(1.,0.,0.));
#7413=DIRECTION('center_axis',(0.,1.,0.));
#7414=DIRECTION('ref_axis',(1.,0.,0.));
#7415=DIRECTION('center_axis',(0.,1.,0.));
#7416=DIRECTION('ref_axis',(1.,0.,0.));
#7417=DIRECTION('center_axis',(0.,-1.,0.));
#7418=DIRECTION('ref_axis',(1.,0.,0.));
#7419=DIRECTION('center_axis',(0.,1.,0.));
#7420=DIRECTION('ref_axis',(1.,0.,0.));
#7421=DIRECTION('center_axis',(0.,1.,0.));
#7422=DIRECTION('ref_axis',(1.,0.,0.));
#7423=DIRECTION('',(0.,-1.,0.));
#7424=DIRECTION('center_axis',(0.,1.,0.));
#7425=DIRECTION('ref_axis',(1.,0.,0.));
#7426=DIRECTION('center_axis',(0.,1.,0.));
#7427=DIRECTION('ref_axis',(1.,0.,0.));
#7428=DIRECTION('center_axis',(0.,-1.,0.));
#7429=DIRECTION('ref_axis',(1.,0.,0.));
#7430=DIRECTION('center_axis',(0.,1.,0.));
#7431=DIRECTION('ref_axis',(1.,0.,0.));
#7432=DIRECTION('',(0.,-1.,0.));
#7433=DIRECTION('center_axis',(0.,1.,0.));
#7434=DIRECTION('ref_axis',(1.,0.,0.));
#7435=DIRECTION('',(0.,-1.,0.));
#7436=DIRECTION('center_axis',(0.,1.,0.));
#7437=DIRECTION('ref_axis',(1.,0.,0.));
#7438=DIRECTION('center_axis',(0.,1.,0.));
#7439=DIRECTION('ref_axis',(1.,0.,0.));
#7440=DIRECTION('center_axis',(0.,1.,0.));
#7441=DIRECTION('ref_axis',(1.,0.,0.));
#7442=DIRECTION('axis',(0.,0.,1.));
#7443=DIRECTION('refdir',(1.,0.,0.));
#7444=DIRECTION('center_axis',(0.,1.,0.));
#7445=DIRECTION('ref_axis',(1.,0.,0.));
#7446=DIRECTION('center_axis',(0.,-1.,0.));
#7447=DIRECTION('ref_axis',(1.,0.,0.));
#7448=DIRECTION('',(0.,-1.,0.));
#7449=DIRECTION('center_axis',(0.,-1.,0.));
#7450=DIRECTION('ref_axis',(1.,0.,0.));
#7451=DIRECTION('center_axis',(0.,1.,0.));
#7452=DIRECTION('ref_axis',(1.,0.,0.));
#7453=DIRECTION('center_axis',(0.,1.,0.));
#7454=DIRECTION('ref_axis',(1.,0.,0.));
#7455=DIRECTION('',(0.,-1.,0.));
#7456=DIRECTION('center_axis',(0.,1.,0.));
#7457=DIRECTION('ref_axis',(1.,0.,0.));
#7458=DIRECTION('center_axis',(0.,1.,0.));
#7459=DIRECTION('ref_axis',(1.,0.,0.));
#7460=DIRECTION('center_axis',(0.,1.,0.));
#7461=DIRECTION('ref_axis',(1.,0.,0.));
#7462=DIRECTION('axis',(0.,0.,1.));
#7463=DIRECTION('refdir',(1.,0.,0.));
#7464=DIRECTION('center_axis',(0.,1.,0.));
#7465=DIRECTION('ref_axis',(1.,0.,0.));
#7466=DIRECTION('center_axis',(0.,-1.,0.));
#7467=DIRECTION('ref_axis',(1.,0.,0.));
#7468=DIRECTION('',(0.,-1.,0.));
#7469=DIRECTION('center_axis',(0.,-1.,0.));
#7470=DIRECTION('ref_axis',(1.,0.,0.));
#7471=DIRECTION('center_axis',(0.,1.,0.));
#7472=DIRECTION('ref_axis',(1.,0.,0.));
#7473=DIRECTION('center_axis',(0.,1.,0.));
#7474=DIRECTION('ref_axis',(1.,0.,0.));
#7475=DIRECTION('',(0.,-1.,0.));
#7476=DIRECTION('center_axis',(0.,1.,0.));
#7477=DIRECTION('ref_axis',(1.,0.,0.));
#7478=DIRECTION('center_axis',(0.,1.,0.));
#7479=DIRECTION('ref_axis',(1.,0.,0.));
#7480=DIRECTION('center_axis',(0.,1.,0.));
#7481=DIRECTION('ref_axis',(1.,0.,0.));
#7482=DIRECTION('axis',(0.,0.,1.));
#7483=DIRECTION('refdir',(1.,0.,0.));
#7484=DIRECTION('center_axis',(0.,0.707106781186548,0.707106781186547));
#7485=DIRECTION('ref_axis',(1.,0.,0.));
#7486=DIRECTION('',(-1.96261557335472E-15,-0.707106781186547,0.707106781186548));
#7487=DIRECTION('',(1.,0.,0.));
#7488=DIRECTION('',(0.,0.707106781186547,-0.707106781186548));
#7489=DIRECTION('',(-1.,0.,0.));
#7490=DIRECTION('center_axis',(0.,0.,-1.));
#7491=DIRECTION('ref_axis',(0.,1.,0.));
#7492=DIRECTION('',(0.,0.707106781186548,0.707106781186548));
#7493=DIRECTION('center_axis',(0.,0.,-1.));
#7494=DIRECTION('ref_axis',(0.,1.,0.));
#7495=DIRECTION('center_axis',(0.,0.,1.));
#7496=DIRECTION('ref_axis',(0.,1.,0.));
#7497=DIRECTION('center_axis',(0.,-0.707106781186548,0.707106781186547));
#7498=DIRECTION('ref_axis',(1.,0.,0.));
#7499=DIRECTION('',(1.96261557335472E-15,0.707106781186547,0.707106781186548));
#7500=DIRECTION('',(-1.,0.,0.));
#7501=DIRECTION('',(1.,0.,0.));
#7502=DIRECTION('center_axis',(0.,0.,-1.));
#7503=DIRECTION('ref_axis',(0.,-1.,0.));
#7504=DIRECTION('center_axis',(0.,0.,-1.));
#7505=DIRECTION('ref_axis',(0.,-1.,0.));
#7506=DIRECTION('center_axis',(0.,0.,1.));
#7507=DIRECTION('ref_axis',(0.,-1.,0.));
#7508=DIRECTION('center_axis',(0.,0.,1.));
#7509=DIRECTION('ref_axis',(0.,1.,0.));
#7510=DIRECTION('',(0.,0.,1.));
#7511=DIRECTION('center_axis',(0.,0.,-1.));
#7512=DIRECTION('ref_axis',(0.,1.,0.));
#7513=DIRECTION('',(0.,0.,1.));
#7514=DIRECTION('center_axis',(0.,1.,0.));
#7515=DIRECTION('ref_axis',(-1.,0.,0.));
#7516=DIRECTION('',(0.,0.,1.));
#7517=DIRECTION('',(1.,0.,0.));
#7518=DIRECTION('center_axis',(0.,0.,1.));
#7519=DIRECTION('ref_axis',(1.,0.,0.));
#7520=DIRECTION('center_axis',(0.,0.707106781186548,-0.707106781186548));
#7521=DIRECTION('ref_axis',(-1.,0.,0.));
#7522=DIRECTION('',(1.96261557335472E-15,0.707106781186548,0.707106781186548));
#7523=DIRECTION('',(0.,-0.707106781186548,-0.707106781186548));
#7524=DIRECTION('',(-1.,0.,0.));
#7525=DIRECTION('center_axis',(0.,0.,1.));
#7526=DIRECTION('ref_axis',(0.,1.,0.));
#7527=DIRECTION('',(0.,-0.707106781186548,0.707106781186547));
#7528=DIRECTION('center_axis',(0.,0.,1.));
#7529=DIRECTION('ref_axis',(0.,1.,0.));
#7530=DIRECTION('center_axis',(0.,-0.707106781186548,-0.707106781186548));
#7531=DIRECTION('ref_axis',(-1.,0.,0.));
#7532=DIRECTION('',(-1.96261557335472E-15,-0.707106781186548,0.707106781186548));
#7533=DIRECTION('',(-1.,0.,0.));
#7534=DIRECTION('',(1.,0.,0.));
#7535=DIRECTION('center_axis',(0.,0.,1.));
#7536=DIRECTION('ref_axis',(0.,-1.,0.));
#7537=DIRECTION('center_axis',(0.,0.,-1.));
#7538=DIRECTION('ref_axis',(0.,-1.,0.));
#7539=DIRECTION('center_axis',(0.,0.,1.));
#7540=DIRECTION('ref_axis',(0.,-1.,0.));
#7541=DIRECTION('center_axis',(0.,0.,1.));
#7542=DIRECTION('ref_axis',(0.,-1.,0.));
#7543=DIRECTION('',(0.,0.,1.));
#7544=DIRECTION('center_axis',(0.,0.,1.));
#7545=DIRECTION('ref_axis',(1.,0.,0.));
#7546=DIRECTION('center_axis',(0.,-1.,0.));
#7547=DIRECTION('ref_axis',(1.,0.,0.));
#7548=DIRECTION('axis',(0.,0.,1.));
#7549=DIRECTION('refdir',(1.,0.,0.));
#7550=DIRECTION('center_axis',(0.866025403784439,0.,-0.5));
#7551=DIRECTION('ref_axis',(0.5,0.,0.866025403784439));
#7552=DIRECTION('',(0.5,0.,0.866025403784439));
#7553=DIRECTION('',(0.,-1.,0.));
#7554=DIRECTION('',(0.5,0.,0.866025403784439));
#7555=DIRECTION('',(0.,-1.,0.));
#7556=DIRECTION('center_axis',(1.92296268638356E-16,0.,-1.));
#7557=DIRECTION('ref_axis',(1.,0.,1.92296268638356E-16));
#7558=DIRECTION('',(1.,0.,1.92296268638356E-16));
#7559=DIRECTION('',(0.,-1.,0.));
#7560=DIRECTION('',(1.,0.,1.92296268638356E-16));
#7561=DIRECTION('center_axis',(-0.866025403784439,0.,-0.5));
#7562=DIRECTION('ref_axis',(0.5,0.,-0.866025403784439));
#7563=DIRECTION('',(0.5,0.,-0.866025403784439));
#7564=DIRECTION('',(0.,-1.,0.));
#7565=DIRECTION('',(0.5,0.,-0.866025403784438));
#7566=DIRECTION('center_axis',(-0.866025403784439,0.,0.5));
#7567=DIRECTION('ref_axis',(-0.5,0.,-0.866025403784439));
#7568=DIRECTION('',(-0.5,0.,-0.866025403784439));
#7569=DIRECTION('',(0.,-1.,0.));
#7570=DIRECTION('',(-0.5,0.,-0.866025403784439));
#7571=DIRECTION('center_axis',(-1.92296268638356E-16,0.,1.));
#7572=DIRECTION('ref_axis',(-1.,0.,-1.92296268638356E-16));
#7573=DIRECTION('',(-1.,0.,-1.92296268638356E-16));
#7574=DIRECTION('',(0.,-1.,0.));
#7575=DIRECTION('',(-1.,0.,-1.92296268638356E-16));
#7576=DIRECTION('center_axis',(0.866025403784439,0.,0.5));
#7577=DIRECTION('ref_axis',(-0.5,0.,0.866025403784439));
#7578=DIRECTION('',(-0.5,0.,0.866025403784439));
#7579=DIRECTION('',(-0.5,0.,0.866025403784439));
#7580=DIRECTION('center_axis',(0.,-1.,0.));
#7581=DIRECTION('ref_axis',(0.,0.,-1.));
#7582=DIRECTION('center_axis',(0.,1.,0.));
#7583=DIRECTION('ref_axis',(0.,0.,1.));
#7584=DIRECTION('center_axis',(0.,-1.,0.));
#7585=DIRECTION('ref_axis',(1.,0.,0.));
#7586=DIRECTION('center_axis',(0.,-1.,0.));
#7587=DIRECTION('ref_axis',(1.,0.,0.));
#7588=DIRECTION('center_axis',(0.,-1.,0.));
#7589=DIRECTION('ref_axis',(1.,0.,0.));
#7590=DIRECTION('',(0.707106781186547,0.707106781186548,8.65956056235493E-17));
#7591=DIRECTION('center_axis',(0.,-1.,0.));
#7592=DIRECTION('ref_axis',(1.,0.,0.));
#7593=DIRECTION('center_axis',(0.,1.,0.));
#7594=DIRECTION('ref_axis',(1.,0.,0.));
#7595=DIRECTION('',(0.,1.,0.));
#7596=DIRECTION('center_axis',(0.,1.,0.));
#7597=DIRECTION('ref_axis',(1.,0.,0.));
#7598=DIRECTION('center_axis',(0.,-1.,0.));
#7599=DIRECTION('ref_axis',(1.,0.,0.));
#7600=DIRECTION('',(-0.707106781186547,0.707106781186548,-8.65956056235493E-17));
#7601=DIRECTION('center_axis',(0.,-1.,0.));
#7602=DIRECTION('ref_axis',(0.,0.,-1.));
#7603=DIRECTION('axis',(0.,0.,1.));
#7604=DIRECTION('refdir',(1.,0.,0.));
#7605=DIRECTION('center_axis',(0.866025403784439,0.,-0.5));
#7606=DIRECTION('ref_axis',(0.5,0.,0.866025403784439));
#7607=DIRECTION('',(-0.5,0.,-0.866025403784439));
#7608=DIRECTION('',(0.,-1.,0.));
#7609=DIRECTION('',(0.5,0.,0.866025403784439));
#7610=DIRECTION('',(0.,-1.,0.));
#7611=DIRECTION('center_axis',(1.60246890531964E-16,0.,-1.));
#7612=DIRECTION('ref_axis',(1.,0.,1.60246890531964E-16));
#7613=DIRECTION('',(-1.,0.,-1.60246890531964E-16));
#7614=DIRECTION('',(0.,-1.,0.));
#7615=DIRECTION('',(1.,0.,1.60246890531964E-16));
#7616=DIRECTION('center_axis',(-0.866025403784439,0.,-0.5));
#7617=DIRECTION('ref_axis',(0.5,0.,-0.866025403784439));
#7618=DIRECTION('',(-0.5,0.,0.866025403784439));
#7619=DIRECTION('',(0.,-1.,0.));
#7620=DIRECTION('',(0.5,0.,-0.866025403784439));
#7621=DIRECTION('center_axis',(-0.866025403784439,0.,0.5));
#7622=DIRECTION('ref_axis',(-0.5,0.,-0.866025403784439));
#7623=DIRECTION('',(0.5,0.,0.866025403784439));
#7624=DIRECTION('',(0.,-1.,0.));
#7625=DIRECTION('',(-0.5,0.,-0.866025403784439));
#7626=DIRECTION('center_axis',(-1.60246890531964E-16,0.,1.));
#7627=DIRECTION('ref_axis',(-1.,0.,-1.60246890531964E-16));
#7628=DIRECTION('',(1.,0.,1.60246890531964E-16));
#7629=DIRECTION('',(0.,-1.,0.));
#7630=DIRECTION('',(-1.,0.,-1.60246890531964E-16));
#7631=DIRECTION('center_axis',(0.866025403784439,0.,0.5));
#7632=DIRECTION('ref_axis',(-0.5,0.,0.866025403784439));
#7633=DIRECTION('',(0.5,0.,-0.866025403784439));
#7634=DIRECTION('',(-0.5,0.,0.866025403784439));
#7635=DIRECTION('center_axis',(0.,1.,0.));
#7636=DIRECTION('ref_axis',(1.,0.,0.));
#7637=DIRECTION('center_axis',(0.,-1.,0.));
#7638=DIRECTION('ref_axis',(0.,0.,-1.));
#7639=DIRECTION('center_axis',(0.,1.,0.));
#7640=DIRECTION('ref_axis',(1.,0.,0.));
#7641=DIRECTION('center_axis',(0.,1.,0.));
#7642=DIRECTION('ref_axis',(1.,0.,0.));
#7643=DIRECTION('center_axis',(0.,1.,0.));
#7644=DIRECTION('ref_axis',(0.,0.,1.));
#7645=DIRECTION('center_axis',(0.,-1.,0.));
#7646=DIRECTION('ref_axis',(1.,0.,0.));
#7647=DIRECTION('center_axis',(0.,-1.,0.));
#7648=DIRECTION('ref_axis',(1.,0.,0.));
#7649=DIRECTION('center_axis',(0.,-1.,0.));
#7650=DIRECTION('ref_axis',(1.,0.,0.));
#7651=DIRECTION('',(0.707106781186547,0.707106781186548,8.65956056235493E-17));
#7652=DIRECTION('center_axis',(0.,-1.,0.));
#7653=DIRECTION('ref_axis',(1.,0.,0.));
#7654=DIRECTION('center_axis',(0.,-1.,0.));
#7655=DIRECTION('ref_axis',(1.,0.,0.));
#7656=DIRECTION('',(0.,1.,0.));
#7657=DIRECTION('center_axis',(0.,1.,0.));
#7658=DIRECTION('ref_axis',(1.,0.,0.));
#7659=DIRECTION('center_axis',(0.,-1.,0.));
#7660=DIRECTION('ref_axis',(1.,0.,0.));
#7661=DIRECTION('',(-0.707106781186547,0.707106781186548,-8.65956056235493E-17));
#7662=DIRECTION('center_axis',(0.,-1.,0.));
#7663=DIRECTION('ref_axis',(0.,0.,-1.));
#7664=DIRECTION('center_axis',(0.,-1.,0.));
#7665=DIRECTION('ref_axis',(1.,0.,0.));
#7666=DIRECTION('center_axis',(0.,1.,0.));
#7667=DIRECTION('ref_axis',(1.,0.,0.));
#7668=DIRECTION('center_axis',(0.,1.,0.));
#7669=DIRECTION('ref_axis',(1.,0.,0.));
#7670=DIRECTION('',(-0.447213595499958,0.894427190999916,-5.47678698264203E-17));
#7671=DIRECTION('center_axis',(0.,-1.,0.));
#7672=DIRECTION('ref_axis',(1.,0.,0.));
#7673=DIRECTION('',(0.,1.,0.));
#7674=DIRECTION('axis',(0.,0.,1.));
#7675=DIRECTION('refdir',(1.,0.,0.));
#7676=DIRECTION('axis',(0.,0.,1.));
#7677=DIRECTION('refdir',(1.,0.,0.));
#7678=DIRECTION('center_axis',(0.,-1.,0.));
#7679=DIRECTION('ref_axis',(0.,0.,-1.));
#7680=DIRECTION('center_axis',(0.,-1.,0.));
#7681=DIRECTION('ref_axis',(1.,0.,0.));
#7682=DIRECTION('center_axis',(0.,-1.,0.));
#7683=DIRECTION('ref_axis',(1.,0.,0.));
#7684=DIRECTION('center_axis',(1.,0.,1.22464679914735E-16));
#7685=DIRECTION('ref_axis',(-1.22464679914735E-16,0.,1.));
#7686=DIRECTION('center_axis',(0.,1.,0.));
#7687=DIRECTION('ref_axis',(1.,0.,0.));
#7688=DIRECTION('center_axis',(0.,1.,0.));
#7689=DIRECTION('ref_axis',(1.,0.,0.));
#7690=DIRECTION('center_axis',(0.,-1.,0.));
#7691=DIRECTION('ref_axis',(1.,0.,0.));
#7692=DIRECTION('',(0.,1.,0.));
#7693=DIRECTION('center_axis',(0.,-1.,0.));
#7694=DIRECTION('ref_axis',(1.,0.,0.));
#7695=DIRECTION('center_axis',(0.,-1.,0.));
#7696=DIRECTION('ref_axis',(1.,0.,0.));
#7697=DIRECTION('center_axis',(0.,-1.,0.));
#7698=DIRECTION('ref_axis',(1.,0.,0.));
#7699=DIRECTION('',(0.,1.,0.));
#7700=DIRECTION('center_axis',(0.,-1.,0.));
#7701=DIRECTION('ref_axis',(1.,0.,0.));
#7702=DIRECTION('center_axis',(0.,1.,0.));
#7703=DIRECTION('ref_axis',(1.,0.,0.));
#7704=DIRECTION('',(-0.707106781186547,0.707106781186548,-8.65956056235493E-17));
#7705=DIRECTION('center_axis',(0.,-1.,0.));
#7706=DIRECTION('ref_axis',(1.,0.,0.));
#7707=DIRECTION('center_axis',(0.,1.,0.));
#7708=DIRECTION('ref_axis',(0.,0.,1.));
#7709=DIRECTION('center_axis',(0.,-1.,0.));
#7710=DIRECTION('ref_axis',(1.,0.,0.));
#7711=DIRECTION('center_axis',(0.,-1.,0.));
#7712=DIRECTION('ref_axis',(1.,0.,0.));
#7713=DIRECTION('',(0.,1.,0.));
#7714=DIRECTION('center_axis',(0.,-1.,0.));
#7715=DIRECTION('ref_axis',(0.,0.,-1.));
#7716=DIRECTION('center_axis',(0.,-1.,0.));
#7717=DIRECTION('ref_axis',(1.,0.,0.));
#7718=DIRECTION('center_axis',(0.,-1.,0.));
#7719=DIRECTION('ref_axis',(1.,0.,0.));
#7720=DIRECTION('',(0.707106781186547,0.707106781186548,8.65956056235493E-17));
#7721=DIRECTION('axis',(0.,0.,1.));
#7722=DIRECTION('refdir',(1.,0.,0.));
#7723=DIRECTION('center_axis',(0.,-1.,0.));
#7724=DIRECTION('ref_axis',(0.,0.,-1.));
#7725=DIRECTION('center_axis',(0.,-1.,0.));
#7726=DIRECTION('ref_axis',(1.,0.,0.));
#7727=DIRECTION('center_axis',(0.,-1.,0.));
#7728=DIRECTION('ref_axis',(1.,0.,0.));
#7729=DIRECTION('center_axis',(1.,0.,1.22464679914735E-16));
#7730=DIRECTION('ref_axis',(-1.22464679914735E-16,0.,1.));
#7731=DIRECTION('center_axis',(0.,1.,0.));
#7732=DIRECTION('ref_axis',(1.,0.,0.));
#7733=DIRECTION('center_axis',(0.,1.,0.));
#7734=DIRECTION('ref_axis',(1.,0.,0.));
#7735=DIRECTION('center_axis',(0.,-1.,0.));
#7736=DIRECTION('ref_axis',(1.,0.,0.));
#7737=DIRECTION('center_axis',(0.,-1.,0.));
#7738=DIRECTION('ref_axis',(1.,0.,0.));
#7739=DIRECTION('',(0.,1.,0.));
#7740=DIRECTION('center_axis',(0.,1.,0.));
#7741=DIRECTION('ref_axis',(0.,0.,1.));
#7742=DIRECTION('center_axis',(0.,-1.,0.));
#7743=DIRECTION('ref_axis',(1.,0.,0.));
#7744=DIRECTION('center_axis',(0.,-1.,0.));
#7745=DIRECTION('ref_axis',(1.,0.,0.));
#7746=DIRECTION('center_axis',(0.,-1.,0.));
#7747=DIRECTION('ref_axis',(1.,0.,0.));
#7748=DIRECTION('center_axis',(0.,-1.,0.));
#7749=DIRECTION('ref_axis',(1.,0.,0.));
#7750=DIRECTION('',(0.707106781186548,0.707106781186547,8.65956056235494E-17));
#7751=DIRECTION('center_axis',(0.,-1.,0.));
#7752=DIRECTION('ref_axis',(1.,0.,0.));
#7753=DIRECTION('center_axis',(0.,-1.,0.));
#7754=DIRECTION('ref_axis',(1.,0.,0.));
#7755=DIRECTION('',(0.,1.,0.));
#7756=DIRECTION('center_axis',(0.,1.,0.));
#7757=DIRECTION('ref_axis',(1.,0.,0.));
#7758=DIRECTION('center_axis',(0.,-1.,0.));
#7759=DIRECTION('ref_axis',(1.,0.,0.));
#7760=DIRECTION('',(-0.707106781186548,0.707106781186547,-8.65956056235494E-17));
#7761=DIRECTION('center_axis',(0.,-1.,0.));
#7762=DIRECTION('ref_axis',(0.,0.,-1.));
#7763=DIRECTION('center_axis',(0.,-1.,0.));
#7764=DIRECTION('ref_axis',(1.,0.,0.));
#7765=DIRECTION('',(0.,1.,0.));
#7766=DIRECTION('axis',(0.,0.,1.));
#7767=DIRECTION('refdir',(1.,0.,0.));
#7768=DIRECTION('center_axis',(0.,0.,1.));
#7769=DIRECTION('ref_axis',(1.,0.,0.));
#7770=DIRECTION('center_axis',(1.22464679914735E-16,-1.,0.));
#7771=DIRECTION('ref_axis',(-1.,-1.22464679914735E-16,0.));
#7772=DIRECTION('center_axis',(0.707106781186548,0.,0.707106781186548));
#7773=DIRECTION('ref_axis',(0.707106781186548,0.,-0.707106781186548));
#7774=DIRECTION('center_axis',(8.65956056235494E-17,-1.,-8.65956056235493E-17));
#7775=DIRECTION('ref_axis',(-0.707106781186547,-1.22464679914735E-16,0.707106781186547));
#7776=DIRECTION('center_axis',(1.,0.,0.));
#7777=DIRECTION('ref_axis',(6.12323399573676E-17,0.,-1.));
#7778=DIRECTION('center_axis',(7.49879891330929E-33,-1.,-1.22464679914735E-16));
#7779=DIRECTION('ref_axis',(-6.12323399573676E-17,-1.22464679914735E-16,
1.));
#7780=DIRECTION('center_axis',(0.707106781186548,0.,-0.707106781186548));
#7781=DIRECTION('ref_axis',(-0.707106781186548,0.,-0.707106781186548));
#7782=DIRECTION('center_axis',(-8.65956056235493E-17,-1.,-8.65956056235494E-17));
#7783=DIRECTION('ref_axis',(0.707106781186547,-1.22464679914735E-16,0.707106781186547));
#7784=DIRECTION('center_axis',(0.,0.,-1.));
#7785=DIRECTION('ref_axis',(-1.,0.,-1.22464679914735E-16));
#7786=DIRECTION('center_axis',(-1.22464679914735E-16,-1.,-1.49975978266186E-32));
#7787=DIRECTION('ref_axis',(1.,-1.22464679914735E-16,1.22464679914735E-16));
#7788=DIRECTION('center_axis',(-0.707106781186547,0.,-0.707106781186548));
#7789=DIRECTION('ref_axis',(-0.707106781186548,0.,0.707106781186547));
#7790=DIRECTION('center_axis',(-8.65956056235493E-17,-1.,8.65956056235493E-17));
#7791=DIRECTION('ref_axis',(0.707106781186548,-1.22464679914735E-16,-0.707106781186547));
#7792=DIRECTION('center_axis',(-1.,0.,0.));
#7793=DIRECTION('ref_axis',(-1.83697019872103E-16,0.,1.));
#7794=DIRECTION('center_axis',(-2.24963967399279E-32,-1.,1.22464679914735E-16));
#7795=DIRECTION('ref_axis',(1.83697019872103E-16,-1.22464679914735E-16,
-1.));
#7796=DIRECTION('center_axis',(-0.707106781186548,0.,0.707106781186548));
#7797=DIRECTION('ref_axis',(0.707106781186547,0.,0.707106781186548));
#7798=DIRECTION('center_axis',(8.65956056235493E-17,-1.,8.65956056235493E-17));
#7799=DIRECTION('ref_axis',(-0.707106781186547,-1.22464679914735E-16,-0.707106781186548));
#7800=DIRECTION('axis',(0.,0.,1.));
#7801=DIRECTION('refdir',(1.,0.,0.));
#7802=DIRECTION('center_axis',(0.,0.,1.));
#7803=DIRECTION('ref_axis',(1.,0.,0.));
#7804=DIRECTION('center_axis',(0.,-1.,0.));
#7805=DIRECTION('ref_axis',(0.,0.,-1.));
#7806=DIRECTION('center_axis',(0.,-1.,0.));
#7807=DIRECTION('ref_axis',(0.,0.,-1.));
#7808=DIRECTION('center_axis',(0.,1.,0.));
#7809=DIRECTION('ref_axis',(1.,0.,0.));
#7810=DIRECTION('center_axis',(0.,1.,0.));
#7811=DIRECTION('ref_axis',(1.,0.,0.));
#7812=DIRECTION('center_axis',(0.,1.,0.));
#7813=DIRECTION('ref_axis',(1.,0.,0.));
#7814=DIRECTION('center_axis',(0.,1.,0.));
#7815=DIRECTION('ref_axis',(1.,0.,0.));
#7816=DIRECTION('',(0.,-1.,0.));
#7817=DIRECTION('center_axis',(0.,-1.,0.));
#7818=DIRECTION('ref_axis',(1.,0.,0.));
#7819=DIRECTION('center_axis',(0.,1.,0.));
#7820=DIRECTION('ref_axis',(1.,0.,0.));
#7821=DIRECTION('center_axis',(0.,1.,0.));
#7822=DIRECTION('ref_axis',(1.,0.,0.));
#7823=DIRECTION('center_axis',(0.,1.,0.));
#7824=DIRECTION('ref_axis',(1.,0.,0.));
#7825=DIRECTION('center_axis',(0.,1.,0.));
#7826=DIRECTION('ref_axis',(1.,0.,0.));
#7827=DIRECTION('center_axis',(0.,1.,0.));
#7828=DIRECTION('ref_axis',(1.,0.,0.));
#7829=DIRECTION('center_axis',(0.,1.,0.));
#7830=DIRECTION('ref_axis',(1.,0.,0.));
#7831=DIRECTION('center_axis',(0.,-1.,0.));
#7832=DIRECTION('ref_axis',(1.,0.,0.));
#7833=DIRECTION('center_axis',(0.,-1.,0.));
#7834=DIRECTION('ref_axis',(0.,0.,-1.));
#7835=DIRECTION('center_axis',(6.12323399573677E-17,0.,1.));
#7836=DIRECTION('ref_axis',(1.,0.,0.));
#7837=DIRECTION('center_axis',(0.,-1.,0.));
#7838=DIRECTION('ref_axis',(0.,0.,-1.));
#7839=DIRECTION('center_axis',(0.,1.,0.));
#7840=DIRECTION('ref_axis',(1.,0.,0.));
#7841=DIRECTION('center_axis',(0.,-1.,0.));
#7842=DIRECTION('ref_axis',(1.,0.,0.));
#7843=DIRECTION('center_axis',(0.,-1.,0.));
#7844=DIRECTION('ref_axis',(0.,0.,-1.));
#7845=DIRECTION('center_axis',(0.,0.,1.));
#7846=DIRECTION('ref_axis',(1.,0.,0.));
#7847=DIRECTION('center_axis',(0.,-1.,0.));
#7848=DIRECTION('ref_axis',(0.,0.,-1.));
#7849=DIRECTION('center_axis',(0.,1.,0.));
#7850=DIRECTION('ref_axis',(1.,0.,0.));
#7851=DIRECTION('center_axis',(0.,-1.,0.));
#7852=DIRECTION('ref_axis',(1.,0.,0.));
#7853=DIRECTION('center_axis',(0.,-1.,0.));
#7854=DIRECTION('ref_axis',(0.,0.,-1.));
#7855=DIRECTION('center_axis',(0.,0.,1.));
#7856=DIRECTION('ref_axis',(1.,0.,0.));
#7857=DIRECTION('center_axis',(0.,-1.,0.));
#7858=DIRECTION('ref_axis',(0.,0.,-1.));
#7859=DIRECTION('center_axis',(0.,1.,0.));
#7860=DIRECTION('ref_axis',(1.,0.,0.));
#7861=DIRECTION('center_axis',(0.,-1.,0.));
#7862=DIRECTION('ref_axis',(1.,0.,0.));
#7863=DIRECTION('center_axis',(0.,-1.,0.));
#7864=DIRECTION('ref_axis',(0.,0.,-1.));
#7865=DIRECTION('center_axis',(0.,0.,1.));
#7866=DIRECTION('ref_axis',(1.,0.,0.));
#7867=DIRECTION('center_axis',(0.,-1.,0.));
#7868=DIRECTION('ref_axis',(0.,0.,-1.));
#7869=DIRECTION('center_axis',(0.,1.,0.));
#7870=DIRECTION('ref_axis',(1.,0.,0.));
#7871=DIRECTION('center_axis',(0.,-1.,0.));
#7872=DIRECTION('ref_axis',(1.,0.,0.));
#7873=DIRECTION('center_axis',(0.,-1.,0.));
#7874=DIRECTION('ref_axis',(0.,0.,-1.));
#7875=DIRECTION('center_axis',(6.12323399573676E-17,0.,1.));
#7876=DIRECTION('ref_axis',(1.,0.,0.));
#7877=DIRECTION('center_axis',(0.,-1.,0.));
#7878=DIRECTION('ref_axis',(0.,0.,-1.));
#7879=DIRECTION('center_axis',(0.,1.,0.));
#7880=DIRECTION('ref_axis',(1.,0.,0.));
#7881=DIRECTION('center_axis',(0.,-1.,0.));
#7882=DIRECTION('ref_axis',(1.,0.,0.));
#7883=DIRECTION('center_axis',(0.,-1.,0.));
#7884=DIRECTION('ref_axis',(0.,0.,-1.));
#7885=DIRECTION('center_axis',(0.,0.,1.));
#7886=DIRECTION('ref_axis',(1.,0.,0.));
#7887=DIRECTION('center_axis',(0.,-1.,0.));
#7888=DIRECTION('ref_axis',(0.,0.,-1.));
#7889=DIRECTION('center_axis',(0.,1.,0.));
#7890=DIRECTION('ref_axis',(1.,0.,0.));
#7891=DIRECTION('center_axis',(0.,1.,0.));
#7892=DIRECTION('ref_axis',(1.,0.,0.));
#7893=DIRECTION('',(0.,1.,0.));
#7894=DIRECTION('center_axis',(0.,-1.,0.));
#7895=DIRECTION('ref_axis',(1.,0.,0.));
#7896=DIRECTION('center_axis',(0.,-1.,0.));
#7897=DIRECTION('ref_axis',(1.,0.,0.));
#7898=DIRECTION('center_axis',(0.,1.,0.));
#7899=DIRECTION('ref_axis',(1.,0.,0.));
#7900=DIRECTION('center_axis',(0.,-1.,0.));
#7901=DIRECTION('ref_axis',(0.,0.,-1.));
#7902=DIRECTION('center_axis',(0.,0.,1.));
#7903=DIRECTION('ref_axis',(1.,0.,0.));
#7904=DIRECTION('center_axis',(0.,-1.,0.));
#7905=DIRECTION('ref_axis',(0.,0.,-1.));
#7906=DIRECTION('center_axis',(0.,-1.,0.));
#7907=DIRECTION('ref_axis',(-1.,0.,0.));
#7908=DIRECTION('center_axis',(0.,1.,0.));
#7909=DIRECTION('ref_axis',(1.,0.,0.));
#7910=DIRECTION('axis',(0.,0.,1.));
#7911=DIRECTION('refdir',(1.,0.,0.));
#7912=DIRECTION('center_axis',(0.,1.,0.));
#7913=DIRECTION('ref_axis',(0.,0.,1.));
#7914=DIRECTION('center_axis',(0.,-1.,0.));
#7915=DIRECTION('ref_axis',(1.,0.,0.));
#7916=DIRECTION('center_axis',(0.,-1.,0.));
#7917=DIRECTION('ref_axis',(1.,0.,0.));
#7918=DIRECTION('center_axis',(0.,-1.,0.));
#7919=DIRECTION('ref_axis',(1.,0.,0.));
#7920=DIRECTION('center_axis',(0.,-1.,0.));
#7921=DIRECTION('ref_axis',(1.,0.,0.));
#7922=DIRECTION('',(0.,1.,0.));
#7923=DIRECTION('center_axis',(0.,-1.,0.));
#7924=DIRECTION('ref_axis',(0.,0.,-1.));
#7925=DIRECTION('center_axis',(0.,-1.,0.));
#7926=DIRECTION('ref_axis',(1.,0.,0.));
#7927=DIRECTION('center_axis',(0.,-1.,0.));
#7928=DIRECTION('ref_axis',(1.,0.,0.));
#7929=DIRECTION('',(0.,1.,0.));
#7930=DIRECTION('center_axis',(0.,1.,0.));
#7931=DIRECTION('ref_axis',(0.,0.,1.));
#7932=DIRECTION('center_axis',(0.,-1.,0.));
#7933=DIRECTION('ref_axis',(1.,0.,0.));
#7934=DIRECTION('center_axis',(0.,-1.,0.));
#7935=DIRECTION('ref_axis',(1.,0.,0.));
#7936=DIRECTION('center_axis',(0.,-1.,0.));
#7937=DIRECTION('ref_axis',(1.,0.,0.));
#7938=DIRECTION('center_axis',(0.,-1.,0.));
#7939=DIRECTION('ref_axis',(1.,0.,0.));
#7940=DIRECTION('',(0.,1.,0.));
#7941=DIRECTION('center_axis',(0.,-1.,0.));
#7942=DIRECTION('ref_axis',(0.,0.,-1.));
#7943=DIRECTION('center_axis',(0.,-1.,0.));
#7944=DIRECTION('ref_axis',(1.,0.,0.));
#7945=DIRECTION('center_axis',(0.,-1.,0.));
#7946=DIRECTION('ref_axis',(1.,0.,0.));
#7947=DIRECTION('',(0.,1.,0.));
#7948=DIRECTION('',(0.,0.,1.));
#7949=DIRECTION('',(1.,0.,0.));
#7950=DIRECTION('',(0.,0.,1.));
#7951=DIRECTION('',(1.,0.,0.));
#7952=DIRECTION('',(0.,0.,1.));
#7953=DIRECTION('',(1.,0.,0.));
#7954=DIRECTION('',(0.,0.,1.));
#7955=DIRECTION('',(1.,0.,0.));
#7956=DIRECTION('',(0.,0.,1.));
#7957=DIRECTION('',(1.,0.,0.));
#7958=DIRECTION('axis',(0.,0.,1.));
#7959=DIRECTION('refdir',(1.,0.,0.));
#7960=DIRECTION('center_axis',(0.,1.,0.));
#7961=DIRECTION('ref_axis',(0.,0.,1.));
#7962=DIRECTION('center_axis',(0.,-1.,0.));
#7963=DIRECTION('ref_axis',(1.,0.,0.));
#7964=DIRECTION('center_axis',(0.,-1.,0.));
#7965=DIRECTION('ref_axis',(1.,0.,0.));
#7966=DIRECTION('center_axis',(0.,-1.,0.));
#7967=DIRECTION('ref_axis',(1.,0.,0.));
#7968=DIRECTION('',(0.707106781186547,0.707106781186548,8.65956056235493E-17));
#7969=DIRECTION('center_axis',(0.,-1.,0.));
#7970=DIRECTION('ref_axis',(1.,0.,0.));
#7971=DIRECTION('center_axis',(0.,-1.,0.));
#7972=DIRECTION('ref_axis',(1.,0.,0.));
#7973=DIRECTION('',(0.,1.,0.));
#7974=DIRECTION('center_axis',(0.,1.,0.));
#7975=DIRECTION('ref_axis',(1.,0.,0.));
#7976=DIRECTION('center_axis',(0.,-1.,0.));
#7977=DIRECTION('ref_axis',(1.,0.,0.));
#7978=DIRECTION('',(-0.707106781186547,0.707106781186548,-8.65956056235493E-17));
#7979=DIRECTION('center_axis',(0.,-1.,0.));
#7980=DIRECTION('ref_axis',(0.,0.,-1.));
#7981=DIRECTION('center_axis',(0.,-1.,0.));
#7982=DIRECTION('ref_axis',(1.,0.,0.));
#7983=DIRECTION('center_axis',(0.,1.,0.));
#7984=DIRECTION('ref_axis',(1.,0.,0.));
#7985=DIRECTION('center_axis',(0.,1.,0.));
#7986=DIRECTION('ref_axis',(1.,0.,0.));
#7987=DIRECTION('',(-0.447213595499958,0.894427190999916,-5.47678698264203E-17));
#7988=DIRECTION('center_axis',(0.,-1.,0.));
#7989=DIRECTION('ref_axis',(1.,0.,0.));
#7990=DIRECTION('center_axis',(0.,1.,0.));
#7991=DIRECTION('ref_axis',(1.,0.,0.));
#7992=DIRECTION('',(0.,1.,0.));
#7993=DIRECTION('center_axis',(0.,1.,0.));
#7994=DIRECTION('ref_axis',(1.,0.,0.));
#7995=DIRECTION('center_axis',(0.,-1.,0.));
#7996=DIRECTION('ref_axis',(1.,0.,0.));
#7997=DIRECTION('',(-0.707106781186547,0.707106781186548,-8.65956056235493E-17));
#7998=DIRECTION('center_axis',(0.,-1.,0.));
#7999=DIRECTION('ref_axis',(0.,0.,-1.));
#8000=DIRECTION('center_axis',(0.866025403784439,0.,-0.5));
#8001=DIRECTION('ref_axis',(0.5,0.,0.866025403784439));
#8002=DIRECTION('',(-0.5,0.,-0.866025403784439));
#8003=DIRECTION('',(0.,-1.,0.));
#8004=DIRECTION('',(0.5,0.,0.866025403784439));
#8005=DIRECTION('',(0.,-1.,0.));
#8006=DIRECTION('center_axis',(1.60246890531964E-16,0.,-1.));
#8007=DIRECTION('ref_axis',(1.,0.,1.60246890531964E-16));
#8008=DIRECTION('',(-1.,0.,-1.60246890531964E-16));
#8009=DIRECTION('',(0.,-1.,0.));
#8010=DIRECTION('',(1.,0.,1.60246890531964E-16));
#8011=DIRECTION('center_axis',(-0.866025403784439,0.,-0.5));
#8012=DIRECTION('ref_axis',(0.5,0.,-0.866025403784439));
#8013=DIRECTION('',(-0.5,0.,0.866025403784439));
#8014=DIRECTION('',(0.,-1.,0.));
#8015=DIRECTION('',(0.5,0.,-0.866025403784439));
#8016=DIRECTION('center_axis',(-0.866025403784439,0.,0.5));
#8017=DIRECTION('ref_axis',(-0.5,0.,-0.866025403784439));
#8018=DIRECTION('',(0.5,0.,0.866025403784439));
#8019=DIRECTION('',(0.,-1.,0.));
#8020=DIRECTION('',(-0.5,0.,-0.866025403784439));
#8021=DIRECTION('center_axis',(-1.60246890531964E-16,0.,1.));
#8022=DIRECTION('ref_axis',(-1.,0.,-1.60246890531964E-16));
#8023=DIRECTION('',(1.,0.,1.60246890531964E-16));
#8024=DIRECTION('',(0.,-1.,0.));
#8025=DIRECTION('',(-1.,0.,-1.60246890531964E-16));
#8026=DIRECTION('center_axis',(0.866025403784439,0.,0.5));
#8027=DIRECTION('ref_axis',(-0.5,0.,0.866025403784439));
#8028=DIRECTION('',(0.5,0.,-0.866025403784439));
#8029=DIRECTION('',(-0.5,0.,0.866025403784439));
#8030=DIRECTION('center_axis',(0.,1.,0.));
#8031=DIRECTION('ref_axis',(1.,0.,0.));
#8032=DIRECTION('center_axis',(0.,-1.,0.));
#8033=DIRECTION('ref_axis',(0.,0.,-1.));
#8034=DIRECTION('',(0.,0.,1.));
#8035=DIRECTION('',(1.,0.,0.));
#8036=DIRECTION('',(0.,0.,1.));
#8037=DIRECTION('',(1.,0.,0.));
#8038=DIRECTION('',(0.,0.,1.));
#8039=DIRECTION('',(1.,0.,0.));
#8040=DIRECTION('',(0.,0.,1.));
#8041=DIRECTION('',(1.,0.,0.));
#8042=DIRECTION('',(0.,0.,1.));
#8043=DIRECTION('',(1.,0.,0.));
#8044=DIRECTION('',(0.,0.,1.));
#8045=DIRECTION('',(1.,0.,0.));
#8046=DIRECTION('',(0.,0.,1.));
#8047=DIRECTION('',(1.,0.,0.));
#8048=DIRECTION('',(0.,-1.,2.22044604925031E-16));
#8049=DIRECTION('',(1.,0.,0.));
#8050=DIRECTION('',(0.,-1.,2.22044604925031E-16));
#8051=DIRECTION('',(1.,0.,0.));
#8052=DIRECTION('',(0.,-1.,2.22044604925031E-16));
#8053=DIRECTION('',(1.,0.,0.));
#8054=DIRECTION('',(0.,-1.,2.22044604925031E-16));
#8055=DIRECTION('',(1.,0.,0.));
#8056=DIRECTION('',(0.,-1.,2.22044604925031E-16));
#8057=DIRECTION('',(1.,0.,0.));
#8058=DIRECTION('',(0.,-1.,2.22044604925031E-16));
#8059=DIRECTION('',(1.,0.,0.));
#8060=DIRECTION('',(0.,-1.,2.22044604925031E-16));
#8061=DIRECTION('',(1.,0.,0.));
#8062=DIRECTION('',(0.,-1.,2.22044604925031E-16));
#8063=DIRECTION('',(1.,0.,0.));
#8064=DIRECTION('',(0.,0.,1.));
#8065=DIRECTION('',(1.,0.,0.));
#8066=DIRECTION('',(0.,0.,1.));
#8067=DIRECTION('',(1.,0.,0.));
#8068=DIRECTION('',(0.,0.,1.));
#8069=DIRECTION('',(-1.,1.22464679914735E-16,0.));
#8070=DIRECTION('',(0.,0.,1.));
#8071=DIRECTION('',(-1.,1.22464679914735E-16,0.));
#8072=DIRECTION('',(0.,0.,1.));
#8073=DIRECTION('',(-1.,1.22464679914735E-16,0.));
#8074=DIRECTION('',(0.,0.,1.));
#8075=DIRECTION('',(-1.,1.22464679914735E-16,0.));
#8076=DIRECTION('',(0.,0.,1.));
#8077=DIRECTION('',(1.,0.,0.));
#8078=DIRECTION('',(0.,0.,1.));
#8079=DIRECTION('',(1.,0.,0.));
#8080=DIRECTION('',(0.,0.,1.));
#8081=DIRECTION('',(1.,0.,0.));
#8082=DIRECTION('',(0.,0.,1.));
#8083=DIRECTION('',(1.,0.,0.));
#8084=DIRECTION('',(0.,0.,1.));
#8085=DIRECTION('',(1.,0.,0.));
#8086=DIRECTION('',(0.,0.,1.));
#8087=DIRECTION('',(1.,0.,0.));
#8088=DIRECTION('',(0.,0.,1.));
#8089=DIRECTION('',(1.,0.,0.));
#8090=DIRECTION('',(0.,0.,1.));
#8091=DIRECTION('',(1.,0.,0.));
#8092=DIRECTION('',(0.,0.,1.));
#8093=DIRECTION('',(1.,0.,0.));
#8094=DIRECTION('',(0.,0.,1.));
#8095=DIRECTION('',(1.,0.,0.));
#8096=DIRECTION('',(0.,0.,1.));
#8097=DIRECTION('',(1.,0.,0.));
#8098=DIRECTION('',(8.65956056235493E-17,-8.65956056235493E-17,-1.));
#8099=DIRECTION('',(2.22044604925031E-16,1.,-8.65956056235494E-17));
#8100=DIRECTION('',(0.,-1.,2.22044604925031E-16));
#8101=DIRECTION('',(1.,0.,0.));
#8102=DIRECTION('',(0.,-1.,2.22044604925031E-16));
#8103=DIRECTION('',(1.,0.,0.));
#8104=DIRECTION('',(0.,0.,1.));
#8105=DIRECTION('',(-1.,1.22464679914735E-16,0.));
#8106=DIRECTION('',(0.,0.,1.));
#8107=DIRECTION('',(-1.,1.22464679914735E-16,0.));
#8108=DIRECTION('',(0.,0.,1.));
#8109=DIRECTION('',(1.,0.,0.));
#8110=DIRECTION('',(0.,0.,1.));
#8111=DIRECTION('',(-1.,1.22464679914735E-16,0.));
#8112=DIRECTION('axis',(0.,0.,1.));
#8113=DIRECTION('refdir',(1.,0.,0.));
#8114=DIRECTION('axis',(0.,0.,1.));
#8115=DIRECTION('refdir',(1.,0.,0.));
#8116=DIRECTION('center_axis',(0.,1.,0.));
#8117=DIRECTION('ref_axis',(1.,0.,0.));
#8118=DIRECTION('center_axis',(0.,1.,0.));
#8119=DIRECTION('ref_axis',(1.,0.,0.));
#8120=DIRECTION('',(0.,1.,0.));
#8121=DIRECTION('center_axis',(0.,-1.,0.));
#8122=DIRECTION('ref_axis',(1.,0.,0.));
#8123=DIRECTION('center_axis',(0.,1.,0.));
#8124=DIRECTION('ref_axis',(1.,0.,0.));
#8125=DIRECTION('center_axis',(0.,1.,0.));
#8126=DIRECTION('ref_axis',(1.,0.,0.));
#8127=DIRECTION('center_axis',(0.,1.,0.));
#8128=DIRECTION('ref_axis',(1.,0.,0.));
#8129=DIRECTION('',(0.,-1.,0.));
#8130=DIRECTION('center_axis',(0.,-1.,0.));
#8131=DIRECTION('ref_axis',(1.,0.,0.));
#8132=DIRECTION('center_axis',(0.,1.,0.));
#8133=DIRECTION('ref_axis',(1.,0.,0.));
#8134=DIRECTION('center_axis',(0.,1.,0.));
#8135=DIRECTION('ref_axis',(1.,0.,0.));
#8136=DIRECTION('',(0.,-1.,0.));
#8137=DIRECTION('center_axis',(0.,1.,0.));
#8138=DIRECTION('ref_axis',(1.,0.,0.));
#8139=DIRECTION('center_axis',(0.,1.,0.));
#8140=DIRECTION('ref_axis',(1.,0.,0.));
#8141=DIRECTION('center_axis',(0.,1.,0.));
#8142=DIRECTION('ref_axis',(1.,0.,0.));
#8143=DIRECTION('axis',(0.,0.,1.));
#8144=DIRECTION('refdir',(1.,0.,0.));
#8145=DIRECTION('center_axis',(0.,1.,0.));
#8146=DIRECTION('ref_axis',(1.,0.,0.));
#8147=DIRECTION('center_axis',(0.,-1.,0.));
#8148=DIRECTION('ref_axis',(1.,0.,0.));
#8149=DIRECTION('',(0.,-1.,0.));
#8150=DIRECTION('center_axis',(0.,-1.,0.));
#8151=DIRECTION('ref_axis',(1.,0.,0.));
#8152=DIRECTION('center_axis',(0.,1.,0.));
#8153=DIRECTION('ref_axis',(1.,0.,0.));
#8154=DIRECTION('center_axis',(0.,1.,0.));
#8155=DIRECTION('ref_axis',(1.,0.,0.));
#8156=DIRECTION('',(0.,-1.,0.));
#8157=DIRECTION('center_axis',(0.,1.,0.));
#8158=DIRECTION('ref_axis',(1.,0.,0.));
#8159=DIRECTION('center_axis',(0.,1.,0.));
#8160=DIRECTION('ref_axis',(1.,0.,0.));
#8161=DIRECTION('center_axis',(0.,1.,0.));
#8162=DIRECTION('ref_axis',(1.,0.,0.));
#8163=DIRECTION('',(0.,0.,1.));
#8164=DIRECTION('',(1.,0.,0.));
#8165=DIRECTION('',(0.,0.,1.));
#8166=DIRECTION('',(1.,0.,0.));
#8167=DIRECTION('',(0.,0.,1.));
#8168=DIRECTION('',(1.,0.,0.));
#8169=DIRECTION('',(0.,0.,1.));
#8170=DIRECTION('',(1.,0.,0.));
#8171=DIRECTION('',(0.,0.,1.));
#8172=DIRECTION('',(1.,0.,0.));
#8173=CARTESIAN_POINT('',(0.,0.,0.));
#8174=CARTESIAN_POINT('',(0.,0.,0.));
#8175=CARTESIAN_POINT('',(0.,0.,0.));
#8176=CARTESIAN_POINT('Origin',(3.3,1.,-0.1));
#8177=CARTESIAN_POINT('',(3.05,1.,0.));
#8178=CARTESIAN_POINT('Origin',(3.3,1.,0.));
#8179=CARTESIAN_POINT('',(3.05,1.,1.));
#8180=CARTESIAN_POINT('',(3.05,1.,-0.1));
#8181=CARTESIAN_POINT('Origin',(3.3,1.,1.));
#8182=CARTESIAN_POINT('Origin',(-3.3,3.,-0.1));
#8183=CARTESIAN_POINT('',(-3.55,3.,0.));
#8184=CARTESIAN_POINT('Origin',(-3.3,3.,0.));
#8185=CARTESIAN_POINT('',(-3.55,3.,1.));
#8186=CARTESIAN_POINT('',(-3.55,3.,-0.1));
#8187=CARTESIAN_POINT('Origin',(-3.3,3.,1.));
#8188=CARTESIAN_POINT('Origin',(-3.3,1.,-0.1));
#8189=CARTESIAN_POINT('',(-3.55,1.,0.));
#8190=CARTESIAN_POINT('Origin',(-3.3,1.,0.));
#8191=CARTESIAN_POINT('',(-3.55,1.,1.));
#8192=CARTESIAN_POINT('',(-3.55,1.,-0.1));
#8193=CARTESIAN_POINT('Origin',(-3.3,1.,1.));
#8194=CARTESIAN_POINT('Origin',(3.3,3.,-0.1));
#8195=CARTESIAN_POINT('',(3.05,3.,0.));
#8196=CARTESIAN_POINT('Origin',(3.3,3.,0.));
#8197=CARTESIAN_POINT('',(3.05,3.,1.));
#8198=CARTESIAN_POINT('',(3.05,3.,-0.1));
#8199=CARTESIAN_POINT('Origin',(3.3,3.,1.));
#8200=CARTESIAN_POINT('Origin',(9.5,7.,0.));
#8201=CARTESIAN_POINT('',(9.5,7.,0.));
#8202=CARTESIAN_POINT('',(-9.5,7.,0.));
#8203=CARTESIAN_POINT('',(9.5,7.,0.));
#8204=CARTESIAN_POINT('',(-9.5,7.,1.));
#8205=CARTESIAN_POINT('',(-9.5,7.,0.));
#8206=CARTESIAN_POINT('',(9.5,7.,1.));
#8207=CARTESIAN_POINT('',(9.5,7.,1.));
#8208=CARTESIAN_POINT('',(9.5,7.,0.));
#8209=CARTESIAN_POINT('Origin',(9.5,-1.,0.));
#8210=CARTESIAN_POINT('',(9.5,-1.,0.));
#8211=CARTESIAN_POINT('',(9.5,-1.,0.));
#8212=CARTESIAN_POINT('',(9.5,-1.,1.));
#8213=CARTESIAN_POINT('',(9.5,-1.,1.));
#8214=CARTESIAN_POINT('',(9.5,-1.,0.));
#8215=CARTESIAN_POINT('Origin',(-9.5,-1.,0.));
#8216=CARTESIAN_POINT('',(-9.5,-1.,0.));
#8217=CARTESIAN_POINT('',(-9.5,-1.,0.));
#8218=CARTESIAN_POINT('',(-9.5,-1.,1.));
#8219=CARTESIAN_POINT('',(-9.5,-1.,1.));
#8220=CARTESIAN_POINT('',(-9.5,-1.,0.));
#8221=CARTESIAN_POINT('Origin',(-9.5,7.,0.));
#8222=CARTESIAN_POINT('',(-9.5,7.,0.));
#8223=CARTESIAN_POINT('',(-9.5,7.,1.));
#8224=CARTESIAN_POINT('Origin',(0.,3.,1.));
#8225=CARTESIAN_POINT('Origin',(0.,3.,0.));
#8226=CARTESIAN_POINT('',(0.,0.,0.));
#8227=CARTESIAN_POINT('Origin',(-7.5,7.,-0.3));
#8228=CARTESIAN_POINT('',(-7.5,7.,-0.3));
#8229=CARTESIAN_POINT('',(-9.5,7.,-0.3));
#8230=CARTESIAN_POINT('',(-7.5,7.,-0.3));
#8231=CARTESIAN_POINT('',(-9.5,7.,0.));
#8232=CARTESIAN_POINT('',(-9.5,7.,-0.3));
#8233=CARTESIAN_POINT('',(-7.5,7.,0.));
#8234=CARTESIAN_POINT('',(-7.5,7.,0.));
#8235=CARTESIAN_POINT('',(-7.5,7.,-0.3));
#8236=CARTESIAN_POINT('Origin',(-7.5,-1.,-0.3));
#8237=CARTESIAN_POINT('',(-7.5,-1.,-0.3));
#8238=CARTESIAN_POINT('',(-7.5,-1.,-0.3));
#8239=CARTESIAN_POINT('',(-7.5,-1.,0.));
#8240=CARTESIAN_POINT('',(-7.5,-1.,0.));
#8241=CARTESIAN_POINT('',(-7.5,-1.,-0.3));
#8242=CARTESIAN_POINT('Origin',(-9.5,-1.,-0.3));
#8243=CARTESIAN_POINT('',(-9.5,-1.,-0.3));
#8244=CARTESIAN_POINT('',(-9.5,-1.,-0.3));
#8245=CARTESIAN_POINT('',(-9.5,-1.,0.));
#8246=CARTESIAN_POINT('',(-9.5,-1.,0.));
#8247=CARTESIAN_POINT('',(-9.5,-1.,-0.3));
#8248=CARTESIAN_POINT('Origin',(-9.5,7.,-0.3));
#8249=CARTESIAN_POINT('',(-9.5,7.,-0.3));
#8250=CARTESIAN_POINT('',(-9.5,7.,0.));
#8251=CARTESIAN_POINT('Origin',(-8.5,3.,0.));
#8252=CARTESIAN_POINT('Origin',(-8.5,3.,-0.3));
#8253=CARTESIAN_POINT('',(0.,0.,0.));
#8254=CARTESIAN_POINT('Origin',(9.5,7.,-0.3));
#8255=CARTESIAN_POINT('',(9.5,7.,-0.3));
#8256=CARTESIAN_POINT('',(7.5,7.,-0.3));
#8257=CARTESIAN_POINT('',(9.5,7.,-0.3));
#8258=CARTESIAN_POINT('',(7.5,7.,0.));
#8259=CARTESIAN_POINT('',(7.5,7.,-0.3));
#8260=CARTESIAN_POINT('',(9.5,7.,0.));
#8261=CARTESIAN_POINT('',(9.5,7.,0.));
#8262=CARTESIAN_POINT('',(9.5,7.,-0.3));
#8263=CARTESIAN_POINT('Origin',(9.5,-1.,-0.3));
#8264=CARTESIAN_POINT('',(9.5,-1.,-0.3));
#8265=CARTESIAN_POINT('',(9.5,-1.,-0.3));
#8266=CARTESIAN_POINT('',(9.5,-1.,0.));
#8267=CARTESIAN_POINT('',(9.5,-1.,0.));
#8268=CARTESIAN_POINT('',(9.5,-1.,-0.3));
#8269=CARTESIAN_POINT('Origin',(7.5,-1.,-0.3));
#8270=CARTESIAN_POINT('',(7.5,-1.,-0.3));
#8271=CARTESIAN_POINT('',(7.5,-1.,-0.3));
#8272=CARTESIAN_POINT('',(7.5,-1.,0.));
#8273=CARTESIAN_POINT('',(7.5,-1.,0.));
#8274=CARTESIAN_POINT('',(7.5,-1.,-0.3));
#8275=CARTESIAN_POINT('Origin',(7.5,7.,-0.3));
#8276=CARTESIAN_POINT('',(7.5,7.,-0.3));
#8277=CARTESIAN_POINT('',(7.5,7.,0.));
#8278=CARTESIAN_POINT('Origin',(8.5,3.,0.));
#8279=CARTESIAN_POINT('Origin',(8.5,3.,-0.3));
#8280=CARTESIAN_POINT('',(0.,0.,0.));
#8281=CARTESIAN_POINT('Origin',(-1.4142135623731,-0.8,8.5857864376269));
#8282=CARTESIAN_POINT('',(-1.5792135623731,-0.7,8.5857864376269));
#8283=CARTESIAN_POINT('Origin',(-1.4142135623731,-0.7,8.5857864376269));
#8284=CARTESIAN_POINT('',(-1.5792135623731,4.7,8.5857864376269));
#8285=CARTESIAN_POINT('',(-1.5792135623731,-0.8,8.5857864376269));
#8286=CARTESIAN_POINT('Origin',(-1.4142135623731,4.7,8.5857864376269));
#8287=CARTESIAN_POINT('Origin',(-1.41421356237309,-0.8,11.4142135623731));
#8288=CARTESIAN_POINT('',(-1.57921356237309,-0.7,11.4142135623731));
#8289=CARTESIAN_POINT('Origin',(-1.41421356237309,-0.7,11.4142135623731));
#8290=CARTESIAN_POINT('',(-1.57921356237309,4.7,11.4142135623731));
#8291=CARTESIAN_POINT('',(-1.57921356237309,-0.8,11.4142135623731));
#8292=CARTESIAN_POINT('Origin',(-1.41421356237309,4.7,11.4142135623731));
#8293=CARTESIAN_POINT('Origin',(1.4142135623731,-0.8,11.4142135623731));
#8294=CARTESIAN_POINT('',(1.2492135623731,-0.7,11.4142135623731));
#8295=CARTESIAN_POINT('Origin',(1.4142135623731,-0.7,11.4142135623731));
#8296=CARTESIAN_POINT('',(1.2492135623731,4.7,11.4142135623731));
#8297=CARTESIAN_POINT('',(1.2492135623731,-0.8,11.4142135623731));
#8298=CARTESIAN_POINT('Origin',(1.4142135623731,4.7,11.4142135623731));
#8299=CARTESIAN_POINT('Origin',(1.41421356237309,-0.8,8.5857864376269));
#8300=CARTESIAN_POINT('',(1.24921356237309,-0.7,8.5857864376269));
#8301=CARTESIAN_POINT('Origin',(1.41421356237309,-0.7,8.5857864376269));
#8302=CARTESIAN_POINT('',(1.24921356237309,4.7,8.5857864376269));
#8303=CARTESIAN_POINT('',(1.24921356237309,-0.8,8.5857864376269));
#8304=CARTESIAN_POINT('Origin',(1.41421356237309,4.7,8.5857864376269));
#8305=CARTESIAN_POINT('Origin',(3.3,1.,0.9));
#8306=CARTESIAN_POINT('',(2.97,1.,1.));
#8307=CARTESIAN_POINT('Origin',(3.3,1.,1.));
#8308=CARTESIAN_POINT('',(2.97,1.,1.8));
#8309=CARTESIAN_POINT('',(2.97,1.,0.9));
#8310=CARTESIAN_POINT('Origin',(3.3,1.,1.8));
#8311=CARTESIAN_POINT('Origin',(-3.3,3.,0.9));
#8312=CARTESIAN_POINT('',(-3.63,3.,1.));
#8313=CARTESIAN_POINT('Origin',(-3.3,3.,1.));
#8314=CARTESIAN_POINT('',(-3.63,3.,1.8));
#8315=CARTESIAN_POINT('',(-3.63,3.,0.9));
#8316=CARTESIAN_POINT('Origin',(-3.3,3.,1.8));
#8317=CARTESIAN_POINT('Origin',(-3.3,1.,0.9));
#8318=CARTESIAN_POINT('',(-3.63,1.,1.));
#8319=CARTESIAN_POINT('Origin',(-3.3,1.,1.));
#8320=CARTESIAN_POINT('',(-3.63,1.,1.8));
#8321=CARTESIAN_POINT('',(-3.63,1.,0.9));
#8322=CARTESIAN_POINT('Origin',(-3.3,1.,1.8));
#8323=CARTESIAN_POINT('Origin',(3.3,3.,0.9));
#8324=CARTESIAN_POINT('',(2.97,3.,1.));
#8325=CARTESIAN_POINT('Origin',(3.3,3.,1.));
#8326=CARTESIAN_POINT('',(2.97,3.,1.8));
#8327=CARTESIAN_POINT('',(2.97,3.,0.9));
#8328=CARTESIAN_POINT('Origin',(3.3,3.,1.8));
#8329=CARTESIAN_POINT('Origin',(0.,-0.8,10.));
#8330=CARTESIAN_POINT('',(-1.6,-0.7,10.));
#8331=CARTESIAN_POINT('Origin',(0.,-0.7,10.));
#8332=CARTESIAN_POINT('',(-1.6,4.7,10.));
#8333=CARTESIAN_POINT('',(-1.6,-0.8,10.));
#8334=CARTESIAN_POINT('Origin',(0.,4.7,10.));
#8335=CARTESIAN_POINT('Origin',(-4.2,-0.7,1.8));
#8336=CARTESIAN_POINT('',(2.5,-0.7,1.8));
#8337=CARTESIAN_POINT('',(2.5,4.7,1.8));
#8338=CARTESIAN_POINT('',(2.5,-0.7,1.8));
#8339=CARTESIAN_POINT('',(4.2,-0.7,1.8));
#8340=CARTESIAN_POINT('',(4.2,-0.7,1.8));
#8341=CARTESIAN_POINT('',(4.2,4.7,1.8));
#8342=CARTESIAN_POINT('',(4.2,-0.7,1.8));
#8343=CARTESIAN_POINT('',(4.2,4.7,1.8));
#8344=CARTESIAN_POINT('Origin',(-4.2,-0.7,1.8));
#8345=CARTESIAN_POINT('',(-2.5,4.7,1.8));
#8346=CARTESIAN_POINT('',(-2.5,-0.7,1.8));
#8347=CARTESIAN_POINT('',(-2.5,2.,1.8));
#8348=CARTESIAN_POINT('',(-4.2,4.7,1.8));
#8349=CARTESIAN_POINT('',(4.2,4.7,1.8));
#8350=CARTESIAN_POINT('',(-4.2,-0.7,1.8));
#8351=CARTESIAN_POINT('',(-4.2,-0.7,1.8));
#8352=CARTESIAN_POINT('',(4.2,-0.7,1.8));
#8353=CARTESIAN_POINT('Origin',(-4.2,-0.7,1.));
#8354=CARTESIAN_POINT('',(-4.2,-0.7,1.));
#8355=CARTESIAN_POINT('',(-4.2,-0.7,1.8));
#8356=CARTESIAN_POINT('',(-4.2,4.7,1.));
#8357=CARTESIAN_POINT('',(-4.2,4.7,1.8));
#8358=CARTESIAN_POINT('',(-4.2,-0.7,1.));
#8359=CARTESIAN_POINT('Origin',(4.2,-0.7,1.8));
#8360=CARTESIAN_POINT('',(4.2,-0.7,1.));
#8361=CARTESIAN_POINT('',(4.2,-0.7,1.));
#8362=CARTESIAN_POINT('',(4.2,4.7,1.));
#8363=CARTESIAN_POINT('',(4.2,-0.7,1.));
#8364=CARTESIAN_POINT('',(4.2,4.7,1.));
#8365=CARTESIAN_POINT('Origin',(-2.5,-0.7,1.));
#8366=CARTESIAN_POINT('',(2.5,-0.7,12.5));
#8367=CARTESIAN_POINT('',(2.5,-0.7,1.));
#8368=CARTESIAN_POINT('',(-2.5,-0.7,12.5));
#8369=CARTESIAN_POINT('',(-2.5,-0.7,12.5));
#8370=CARTESIAN_POINT('',(-2.5,-0.7,1.));
#8371=CARTESIAN_POINT('',(-4.2,-0.7,1.));
#8372=CARTESIAN_POINT('Origin',(2.5,-0.7,1.));
#8373=CARTESIAN_POINT('',(2.5,4.7,12.5));
#8374=CARTESIAN_POINT('',(2.5,4.7,1.));
#8375=CARTESIAN_POINT('',(2.5,-0.7,12.5));
#8376=CARTESIAN_POINT('Origin',(2.5,4.7,1.));
#8377=CARTESIAN_POINT('',(-2.5,4.7,12.5));
#8378=CARTESIAN_POINT('',(-2.5,4.7,1.));
#8379=CARTESIAN_POINT('',(2.5,4.7,12.5));
#8380=CARTESIAN_POINT('',(-4.2,4.7,1.));
#8381=CARTESIAN_POINT('Origin',(-2.5,4.7,1.));
#8382=CARTESIAN_POINT('',(-2.5,4.7,12.5));
#8383=CARTESIAN_POINT('Origin',(0.,2.,12.5));
#8384=CARTESIAN_POINT('Origin',(0.,2.,1.));
#8385=CARTESIAN_POINT('',(0.,0.,0.));
#8386=CARTESIAN_POINT('Origin',(0.,0.5,10.));
#8387=CARTESIAN_POINT('',(-1.2,3.5,10.));
#8388=CARTESIAN_POINT('Origin',(0.,3.5,10.));
#8389=CARTESIAN_POINT('',(-1.2,0.5,10.));
#8390=CARTESIAN_POINT('',(-1.2,0.5,10.));
#8391=CARTESIAN_POINT('Origin',(0.,0.5,10.));
#8392=CARTESIAN_POINT('Origin',(0.,0.5,10.));
#8393=CARTESIAN_POINT('',(-1.59,3.5,10.));
#8394=CARTESIAN_POINT('Origin',(0.,3.5,10.));
#8395=CARTESIAN_POINT('',(-1.59,0.5,10.));
#8396=CARTESIAN_POINT('',(-1.59,0.5,10.));
#8397=CARTESIAN_POINT('Origin',(0.,0.5,10.));
#8398=CARTESIAN_POINT('Origin',(0.,3.5,10.));
#8399=CARTESIAN_POINT('Origin',(0.,0.5,10.));
#8400=CARTESIAN_POINT('',(0.,0.,0.));
#8401=CARTESIAN_POINT('Origin',(-1.4142135623731,-1.,8.5857864376269));
#8402=CARTESIAN_POINT('',(-1.6392135623731,-0.9,8.5857864376269));
#8403=CARTESIAN_POINT('Origin',(-1.4142135623731,-0.9,8.5857864376269));
#8404=CARTESIAN_POINT('',(-1.6392135623731,-0.7,8.5857864376269));
#8405=CARTESIAN_POINT('',(-1.6392135623731,-1.,8.5857864376269));
#8406=CARTESIAN_POINT('Origin',(-1.4142135623731,-0.7,8.5857864376269));
#8407=CARTESIAN_POINT('Origin',(-1.41421356237309,-1.,11.4142135623731));
#8408=CARTESIAN_POINT('',(-1.6392135623731,-0.9,11.4142135623731));
#8409=CARTESIAN_POINT('Origin',(-1.41421356237309,-0.9,11.4142135623731));
#8410=CARTESIAN_POINT('',(-1.6392135623731,-0.7,11.4142135623731));
#8411=CARTESIAN_POINT('',(-1.6392135623731,-1.,11.4142135623731));
#8412=CARTESIAN_POINT('Origin',(-1.41421356237309,-0.7,11.4142135623731));
#8413=CARTESIAN_POINT('Origin',(1.4142135623731,-1.,11.4142135623731));
#8414=CARTESIAN_POINT('',(1.1892135623731,-0.9,11.4142135623731));
#8415=CARTESIAN_POINT('Origin',(1.4142135623731,-0.9,11.4142135623731));
#8416=CARTESIAN_POINT('',(1.1892135623731,-0.7,11.4142135623731));
#8417=CARTESIAN_POINT('',(1.1892135623731,-1.,11.4142135623731));
#8418=CARTESIAN_POINT('Origin',(1.4142135623731,-0.7,11.4142135623731));
#8419=CARTESIAN_POINT('Origin',(1.41421356237309,-1.,8.5857864376269));
#8420=CARTESIAN_POINT('',(1.18921356237309,-0.9,8.5857864376269));
#8421=CARTESIAN_POINT('Origin',(1.41421356237309,-0.9,8.5857864376269));
#8422=CARTESIAN_POINT('',(1.18921356237309,-0.7,8.5857864376269));
#8423=CARTESIAN_POINT('',(1.18921356237309,-1.,8.5857864376269));
#8424=CARTESIAN_POINT('Origin',(1.41421356237309,-0.7,8.5857864376269));
#8425=CARTESIAN_POINT('Origin',(0.,-0.7,10.));
#8426=CARTESIAN_POINT('',(-1.59,-0.5,10.));
#8427=CARTESIAN_POINT('Origin',(0.,-0.5,10.));
#8428=CARTESIAN_POINT('',(-1.59,-0.7,10.));
#8429=CARTESIAN_POINT('',(-1.59,-0.7,10.));
#8430=CARTESIAN_POINT('Origin',(0.,-0.7,10.));
#8431=CARTESIAN_POINT('Origin',(0.,-0.5,10.));
#8432=CARTESIAN_POINT('',(-1.2,-0.5,10.));
#8433=CARTESIAN_POINT('Origin',(0.,-0.5,10.));
#8434=CARTESIAN_POINT('Origin',(0.,-0.9,10.));
#8435=CARTESIAN_POINT('',(-1.2,-0.9,10.));
#8436=CARTESIAN_POINT('',(-1.2,-0.9,10.));
#8437=CARTESIAN_POINT('Origin',(0.,-0.9,10.));
#8438=CARTESIAN_POINT('Origin',(0.,-0.9,10.));
#8439=CARTESIAN_POINT('',(-2.4,-0.7,10.));
#8440=CARTESIAN_POINT('Origin',(0.,-0.7,10.));
#8441=CARTESIAN_POINT('',(-2.4,-0.9,10.));
#8442=CARTESIAN_POINT('',(-2.4,-0.9,10.));
#8443=CARTESIAN_POINT('Origin',(0.,-0.9,10.));
#8444=CARTESIAN_POINT('Origin',(0.,-0.7,10.));
#8445=CARTESIAN_POINT('Origin',(0.,-0.9,10.));
#8446=CARTESIAN_POINT('',(0.,0.,0.));
#8447=CARTESIAN_POINT('Origin',(-1.4142135623731,4.4,8.5857864376269));
#8448=CARTESIAN_POINT('',(-1.6392135623731,4.7,8.5857864376269));
#8449=CARTESIAN_POINT('Origin',(-1.4142135623731,4.7,8.5857864376269));
#8450=CARTESIAN_POINT('',(-1.6392135623731,4.9,8.5857864376269));
#8451=CARTESIAN_POINT('',(-1.6392135623731,4.4,8.5857864376269));
#8452=CARTESIAN_POINT('Origin',(-1.4142135623731,4.9,8.5857864376269));
#8453=CARTESIAN_POINT('Origin',(-1.41421356237309,4.4,11.4142135623731));
#8454=CARTESIAN_POINT('',(-1.6392135623731,4.7,11.4142135623731));
#8455=CARTESIAN_POINT('Origin',(-1.41421356237309,4.7,11.4142135623731));
#8456=CARTESIAN_POINT('',(-1.6392135623731,4.9,11.4142135623731));
#8457=CARTESIAN_POINT('',(-1.6392135623731,4.4,11.4142135623731));
#8458=CARTESIAN_POINT('Origin',(-1.41421356237309,4.9,11.4142135623731));
#8459=CARTESIAN_POINT('Origin',(1.4142135623731,4.4,11.4142135623731));
#8460=CARTESIAN_POINT('',(1.1892135623731,4.7,11.4142135623731));
#8461=CARTESIAN_POINT('Origin',(1.4142135623731,4.7,11.4142135623731));
#8462=CARTESIAN_POINT('',(1.1892135623731,4.9,11.4142135623731));
#8463=CARTESIAN_POINT('',(1.1892135623731,4.4,11.4142135623731));
#8464=CARTESIAN_POINT('Origin',(1.4142135623731,4.9,11.4142135623731));
#8465=CARTESIAN_POINT('Origin',(1.41421356237309,4.4,8.5857864376269));
#8466=CARTESIAN_POINT('',(1.18921356237309,4.7,8.5857864376269));
#8467=CARTESIAN_POINT('Origin',(1.41421356237309,4.7,8.5857864376269));
#8468=CARTESIAN_POINT('',(1.18921356237309,4.9,8.5857864376269));
#8469=CARTESIAN_POINT('',(1.18921356237309,4.4,8.5857864376269));
#8470=CARTESIAN_POINT('Origin',(1.41421356237309,4.9,8.5857864376269));
#8471=CARTESIAN_POINT('Origin',(0.,4.5,10.));
#8472=CARTESIAN_POINT('',(-1.59,4.7,10.));
#8473=CARTESIAN_POINT('Origin',(0.,4.7,10.));
#8474=CARTESIAN_POINT('',(-1.59,4.5,10.));
#8475=CARTESIAN_POINT('',(-1.59,4.5,10.));
#8476=CARTESIAN_POINT('Origin',(0.,4.5,10.));
#8477=CARTESIAN_POINT('Origin',(0.,4.5,10.));
#8478=CARTESIAN_POINT('',(-1.2,4.5,10.));
#8479=CARTESIAN_POINT('Origin',(0.,4.5,10.));
#8480=CARTESIAN_POINT('Origin',(0.,4.7,10.));
#8481=CARTESIAN_POINT('',(-1.2,4.9,10.));
#8482=CARTESIAN_POINT('Origin',(0.,4.9,10.));
#8483=CARTESIAN_POINT('',(-1.2,4.7,10.));
#8484=CARTESIAN_POINT('Origin',(0.,4.7,10.));
#8485=CARTESIAN_POINT('',(-2.4,4.9,10.));
#8486=CARTESIAN_POINT('Origin',(0.,4.9,10.));
#8487=CARTESIAN_POINT('',(-2.4,4.7,10.));
#8488=CARTESIAN_POINT('',(-2.4,4.7,10.));
#8489=CARTESIAN_POINT('Origin',(0.,4.7,10.));
#8490=CARTESIAN_POINT('Origin',(0.,4.9,10.));
#8491=CARTESIAN_POINT('Origin',(0.,4.7,10.));
#8492=CARTESIAN_POINT('',(0.,0.,0.));
#8493=CARTESIAN_POINT('Origin',(0.,0.,0.));
#8494=CARTESIAN_POINT('',(-0.32,0.16,3.91886975727153E-17));
#8495=CARTESIAN_POINT('Origin',(0.,0.16,0.));
#8496=CARTESIAN_POINT('',(-0.32,0.,3.91886975727153E-17));
#8497=CARTESIAN_POINT('',(-0.32,0.,3.91886975727153E-17));
#8498=CARTESIAN_POINT('Origin',(0.,0.,0.));
#8499=CARTESIAN_POINT('Origin',(0.,0.,0.));
#8500=CARTESIAN_POINT('',(-0.6,0.16,7.34788079488412E-17));
#8501=CARTESIAN_POINT('Origin',(0.,0.16,0.));
#8502=CARTESIAN_POINT('',(-0.6,0.,7.34788079488412E-17));
#8503=CARTESIAN_POINT('',(-0.6,0.,7.34788079488412E-17));
#8504=CARTESIAN_POINT('Origin',(0.,0.,0.));
#8505=CARTESIAN_POINT('Origin',(0.,0.16,0.));
#8506=CARTESIAN_POINT('Origin',(0.,0.,0.));
#8507=CARTESIAN_POINT('',(0.,0.,0.));
#8508=CARTESIAN_POINT('Origin',(0.144337567297406,-0.6,-0.25));
#8509=CARTESIAN_POINT('',(0.288675134594813,-0.6,0.));
#8510=CARTESIAN_POINT('',(0.144337567297406,-0.6,-0.25));
#8511=CARTESIAN_POINT('',(0.288675134594813,-0.6,0.));
#8512=CARTESIAN_POINT('',(0.144337567297406,-0.96,-0.25));
#8513=CARTESIAN_POINT('',(0.144337567297406,-0.6,-0.25));
#8514=CARTESIAN_POINT('',(0.288675134594813,-0.96,0.));
#8515=CARTESIAN_POINT('',(0.288675134594813,-0.96,0.));
#8516=CARTESIAN_POINT('',(0.288675134594813,-0.6,0.));
#8517=CARTESIAN_POINT('Origin',(-0.144337567297406,-0.6,-0.25));
#8518=CARTESIAN_POINT('',(-0.144337567297406,-0.6,-0.25));
#8519=CARTESIAN_POINT('',(0.144337567297406,-0.6,-0.25));
#8520=CARTESIAN_POINT('',(-0.144337567297406,-0.96,-0.25));
#8521=CARTESIAN_POINT('',(-0.144337567297406,-0.6,-0.25));
#8522=CARTESIAN_POINT('',(0.144337567297406,-0.96,-0.25));
#8523=CARTESIAN_POINT('Origin',(-0.288675134594813,-0.6,-8.32667268468867E-17));
#8524=CARTESIAN_POINT('',(-0.288675134594813,-0.6,-3.53525079574969E-17));
#8525=CARTESIAN_POINT('',(-0.144337567297406,-0.6,-0.25));
#8526=CARTESIAN_POINT('',(-0.288675134594813,-0.96,-5.55111512312578E-17));
#8527=CARTESIAN_POINT('',(-0.288675134594813,-0.6,-3.53525079574969E-17));
#8528=CARTESIAN_POINT('',(-0.144337567297406,-0.96,-0.25));
#8529=CARTESIAN_POINT('Origin',(-0.144337567297407,-0.6,0.25));
#8530=CARTESIAN_POINT('',(-0.144337567297407,-0.6,0.25));
#8531=CARTESIAN_POINT('',(-0.288675134594813,-0.6,-3.53525079574969E-17));
#8532=CARTESIAN_POINT('',(-0.144337567297407,-0.96,0.25));
#8533=CARTESIAN_POINT('',(-0.144337567297407,-0.6,0.25));
#8534=CARTESIAN_POINT('',(-0.288675134594813,-0.96,-3.53525079574969E-17));
#8535=CARTESIAN_POINT('Origin',(0.144337567297406,-0.6,0.25));
#8536=CARTESIAN_POINT('',(0.144337567297406,-0.6,0.25));
#8537=CARTESIAN_POINT('',(-0.144337567297407,-0.6,0.25));
#8538=CARTESIAN_POINT('',(0.144337567297406,-0.96,0.25));
#8539=CARTESIAN_POINT('',(0.144337567297406,-0.6,0.25));
#8540=CARTESIAN_POINT('',(-0.144337567297407,-0.96,0.25));
#8541=CARTESIAN_POINT('Origin',(0.288675134594813,-0.6,0.));
#8542=CARTESIAN_POINT('',(0.144337567297406,-0.6,0.25));
#8543=CARTESIAN_POINT('',(0.144337567297406,-0.96,0.25));
#8544=CARTESIAN_POINT('Origin',(0.,-0.6,0.));
#8545=CARTESIAN_POINT('Origin',(0.,-0.96,0.));
#8546=CARTESIAN_POINT('Origin',(0.,-1.8,0.));
#8547=CARTESIAN_POINT('',(-0.2942,-1.8,3.60291088309151E-17));
#8548=CARTESIAN_POINT('Origin',(0.,-1.8,0.));
#8549=CARTESIAN_POINT('Origin',(0.45,0.6,0.));
#8550=CARTESIAN_POINT('',(-0.45,0.6,-5.51091059616309E-17));
#8551=CARTESIAN_POINT('Origin',(0.,0.6,0.));
#8552=CARTESIAN_POINT('Origin',(0.,0.575,0.));
#8553=CARTESIAN_POINT('',(-0.5,0.55,-6.12323399573677E-17));
#8554=CARTESIAN_POINT('Origin',(0.,0.55,0.));
#8555=CARTESIAN_POINT('',(-0.475,0.575,-5.81707229594993E-17));
#8556=CARTESIAN_POINT('Origin',(0.,0.29,0.));
#8557=CARTESIAN_POINT('',(-0.5,0.0299999999999998,-6.12323399573677E-17));
#8558=CARTESIAN_POINT('Origin',(0.,0.0299999999999998,0.));
#8559=CARTESIAN_POINT('',(-0.5,0.29,-6.12323399573677E-17));
#8560=CARTESIAN_POINT('Origin',(0.,0.0150000000000001,0.));
#8561=CARTESIAN_POINT('',(-0.47,7.11236625150491E-17,-5.75583995599256E-17));
#8562=CARTESIAN_POINT('Origin',(0.,0.,0.));
#8563=CARTESIAN_POINT('',(-0.485,0.0150000000000001,-5.93953697586466E-17));
#8564=CARTESIAN_POINT('Origin',(0.32,0.,0.));
#8565=CARTESIAN_POINT('',(-0.32,-6.93889390390723E-18,-3.91886975727153E-17));
#8566=CARTESIAN_POINT('Origin',(0.,0.,0.));
#8567=CARTESIAN_POINT('Origin',(0.,-0.02,0.));
#8568=CARTESIAN_POINT('',(-0.2942,-0.0515999999999999,3.60291088309151E-17));
#8569=CARTESIAN_POINT('Origin',(0.,-0.0515999999999999,0.));
#8570=CARTESIAN_POINT('',(-0.31,-0.02,-3.7964050773568E-17));
#8571=CARTESIAN_POINT('Origin',(0.,-1.24,0.));
#8572=CARTESIAN_POINT('',(-0.2942,-1.24,-3.60291088309151E-17));
#8573=CARTESIAN_POINT('',(0.,0.,0.));
#8574=CARTESIAN_POINT('',(0.,0.,0.));
#8575=CARTESIAN_POINT('Origin',(0.,0.,0.));
#8576=CARTESIAN_POINT('',(-1.070235,-0.308121667383195,-1.31065986708547E-16));
#8577=CARTESIAN_POINT('',(-1.31065986708547E-16,-0.308121667383195,1.070235));
#8578=CARTESIAN_POINT('Origin',(0.,-0.308121667383195,0.));
#8579=CARTESIAN_POINT('Origin',(0.,-0.308121667383195,0.));
#8580=CARTESIAN_POINT('',(-1.31065986708547E-16,0.308121667383195,1.070235));
#8581=CARTESIAN_POINT('Origin',(-1.34711147906209E-16,0.,1.1));
#8582=CARTESIAN_POINT('',(-1.070235,0.308121667383195,1.31065986708547E-16));
#8583=CARTESIAN_POINT('Origin',(0.,0.308121667383195,0.));
#8584=CARTESIAN_POINT('Origin',(0.,0.308121667383195,0.));
#8585=CARTESIAN_POINT('Origin',(0.,0.,0.));
#8586=CARTESIAN_POINT('',(-1.070235,0.5,-1.31065986708547E-16));
#8587=CARTESIAN_POINT('',(-1.070235,0.,-1.31065986708547E-16));
#8588=CARTESIAN_POINT('Origin',(0.,0.5,0.));
#8589=CARTESIAN_POINT('Origin',(0.,0.,0.));
#8590=CARTESIAN_POINT('',(-0.6,-0.44,-7.34788079488412E-17));
#8591=CARTESIAN_POINT('Origin',(0.,-0.44,0.));
#8592=CARTESIAN_POINT('',(-0.6,0.44,-7.34788079488412E-17));
#8593=CARTESIAN_POINT('',(-0.6,0.,-7.34788079488412E-17));
#8594=CARTESIAN_POINT('Origin',(0.,0.44,0.));
#8595=CARTESIAN_POINT('Origin',(0.,0.47,0.));
#8596=CARTESIAN_POINT('',(-0.66,0.5,-8.08266887437253E-17));
#8597=CARTESIAN_POINT('',(-0.63,0.47,-7.71527483462832E-17));
#8598=CARTESIAN_POINT('Origin',(0.,0.5,0.));
#8599=CARTESIAN_POINT('Origin',(1.070235,0.5,0.));
#8600=CARTESIAN_POINT('Origin',(0.,0.,0.));
#8601=CARTESIAN_POINT('',(-1.070235,-0.5,-1.31065986708547E-16));
#8602=CARTESIAN_POINT('Origin',(0.,-0.5,0.));
#8603=CARTESIAN_POINT('',(-1.070235,0.,-1.31065986708547E-16));
#8604=CARTESIAN_POINT('Origin',(0.66,-0.5,0.));
#8605=CARTESIAN_POINT('',(-0.66,-0.5,-8.08266887437253E-17));
#8606=CARTESIAN_POINT('Origin',(0.,-0.5,0.));
#8607=CARTESIAN_POINT('Origin',(0.,-0.47,0.));
#8608=CARTESIAN_POINT('',(-0.63,-0.47,-7.71527483462832E-17));
#8609=CARTESIAN_POINT('',(0.,0.,0.));
#8610=CARTESIAN_POINT('Origin',(0.,0.,0.));
#8611=CARTESIAN_POINT('',(-1.129765,0.308121667383195,-1.38356309103871E-16));
#8612=CARTESIAN_POINT('',(-1.38356309103871E-16,0.308121667383195,1.129765));
#8613=CARTESIAN_POINT('Origin',(0.,0.308121667383195,0.));
#8614=CARTESIAN_POINT('Origin',(0.,0.308121667383195,0.));
#8615=CARTESIAN_POINT('',(-1.38356309103871E-16,-0.308121667383195,1.129765));
#8616=CARTESIAN_POINT('Origin',(-1.34711147906209E-16,0.,1.1));
#8617=CARTESIAN_POINT('',(-1.129765,-0.308121667383195,1.38356309103871E-16));
#8618=CARTESIAN_POINT('Origin',(0.,-0.308121667383195,0.));
#8619=CARTESIAN_POINT('Origin',(0.,-0.308121667383195,0.));
#8620=CARTESIAN_POINT('Origin',(0.,0.,0.));
#8621=CARTESIAN_POINT('',(-1.129765,-0.5,-1.38356309103871E-16));
#8622=CARTESIAN_POINT('Origin',(0.,-0.5,0.));
#8623=CARTESIAN_POINT('',(-1.129765,0.,-1.38356309103871E-16));
#8624=CARTESIAN_POINT('Origin',(1.54,0.5,0.));
#8625=CARTESIAN_POINT('',(-1.54,0.5,-1.88595607068692E-16));
#8626=CARTESIAN_POINT('Origin',(0.,0.5,0.));
#8627=CARTESIAN_POINT('',(-1.129765,0.5,-1.38356309103871E-16));
#8628=CARTESIAN_POINT('Origin',(0.,0.5,0.));
#8629=CARTESIAN_POINT('Origin',(0.,0.47,0.));
#8630=CARTESIAN_POINT('',(-1.6,0.44,-1.95943487863577E-16));
#8631=CARTESIAN_POINT('Origin',(0.,0.44,0.));
#8632=CARTESIAN_POINT('',(-1.57,0.47,-1.92269547466134E-16));
#8633=CARTESIAN_POINT('Origin',(0.,0.,0.));
#8634=CARTESIAN_POINT('',(-1.6,-0.44,-1.95943487863577E-16));
#8635=CARTESIAN_POINT('Origin',(0.,-0.44,0.));
#8636=CARTESIAN_POINT('',(-1.6,0.,-1.95943487863577E-16));
#8637=CARTESIAN_POINT('Origin',(0.,-0.47,0.));
#8638=CARTESIAN_POINT('',(-1.54,-0.5,-1.88595607068692E-16));
#8639=CARTESIAN_POINT('Origin',(0.,-0.5,0.));
#8640=CARTESIAN_POINT('',(-1.57,-0.47,-1.92269547466134E-16));
#8641=CARTESIAN_POINT('Origin',(1.129765,-0.5,0.));
#8642=CARTESIAN_POINT('Origin',(0.,0.,0.));
#8643=CARTESIAN_POINT('',(-1.129765,0.,-1.38356309103871E-16));
#8644=CARTESIAN_POINT('',(0.,0.,0.));
#8645=CARTESIAN_POINT('Origin',(1.1,0.,0.));
#8646=CARTESIAN_POINT('',(1.1,-2.23201749654651E-33,0.29765));
#8647=CARTESIAN_POINT('',(1.1,-2.23201749654651E-33,-0.29765));
#8648=CARTESIAN_POINT('Origin',(1.1,0.,0.));
#8649=CARTESIAN_POINT('Origin',(0.685838782044607,0.,-0.860014630714833));
#8650=CARTESIAN_POINT('',(0.918550922801216,-5.31350540756609E-33,-0.674432891191581));
#8651=CARTESIAN_POINT('',(0.453126641287998,8.49470414473068E-34,-1.04559637023808));
#8652=CARTESIAN_POINT('Origin',(0.685838782044607,0.,-0.860014630714833));
#8653=CARTESIAN_POINT('Origin',(-0.244773027351946,0.,-1.07242070340001));
#8654=CARTESIAN_POINT('',(0.0454142657089739,-2.23201749654651E-33,-1.1386540593921));
#8655=CARTESIAN_POINT('',(-0.534960320412865,-2.23201749654651E-33,-1.00618734740791));
#8656=CARTESIAN_POINT('Origin',(-0.244773027351946,0.,-1.07242070340001));
#8657=CARTESIAN_POINT('Origin',(-0.991065754692661,0.,-0.477272113029314));
#8658=CARTESIAN_POINT('',(-0.86192025974432,8.49470414473067E-34,-0.745445496560469));
#8659=CARTESIAN_POINT('',(-1.120211249641,-5.31350540756609E-33,-0.209098729498159));
#8660=CARTESIAN_POINT('Origin',(-0.991065754692661,0.,-0.477272113029314));
#8661=CARTESIAN_POINT('Origin',(-0.991065754692661,0.,0.477272113029314));
#8662=CARTESIAN_POINT('',(-1.120211249641,-2.23201749654651E-33,0.209098729498159));
#8663=CARTESIAN_POINT('',(-0.86192025974432,-2.23201749654651E-33,0.745445496560469));
#8664=CARTESIAN_POINT('Origin',(-0.991065754692661,0.,0.477272113029314));
#8665=CARTESIAN_POINT('Origin',(-0.244773027351946,0.,1.07242070340001));
#8666=CARTESIAN_POINT('',(-0.534960320412866,-2.23201749654651E-33,1.00618734740791));
#8667=CARTESIAN_POINT('',(0.0454142657089737,-2.23201749654651E-33,1.1386540593921));
#8668=CARTESIAN_POINT('Origin',(-0.244773027351946,0.,1.07242070340001));
#8669=CARTESIAN_POINT('Origin',(0.685838782044607,0.,0.860014630714833));
#8670=CARTESIAN_POINT('',(0.453126641287998,-2.23201749654651E-33,1.04559637023808));
#8671=CARTESIAN_POINT('',(0.918550922801216,-2.23201749654651E-33,0.674432891191581));
#8672=CARTESIAN_POINT('Origin',(0.685838782044607,0.,0.860014630714833));
#8673=CARTESIAN_POINT('',(0.,0.,0.));
#8674=CARTESIAN_POINT('Origin',(0.685838782044607,0.,0.860014630714833));
#8675=CARTESIAN_POINT('',(0.413083465285518,-0.05953,0.993751811093549));
#8676=CARTESIAN_POINT('',(0.876916659919095,-0.05953,0.623857181492959));
#8677=CARTESIAN_POINT('Ctrl Pts',(0.413083465285518,-0.05953,0.993751811093549));
#8678=CARTESIAN_POINT('Ctrl Pts',(0.419070565453383,-0.0925528133349865,
0.991263089003441));
#8679=CARTESIAN_POINT('Ctrl Pts',(0.430199341854858,-0.124911173756694,
0.986608710139579));
#8680=CARTESIAN_POINT('Ctrl Pts',(0.457978755888596,-0.177924977804098,
0.973971221090534));
#8681=CARTESIAN_POINT('Ctrl Pts',(0.473077587363685,-0.199697230012983,
0.966820759530997));
#8682=CARTESIAN_POINT('Ctrl Pts',(0.507057380724533,-0.237895043532788,
0.949440676105255));
#8683=CARTESIAN_POINT('Ctrl Pts',(0.525933334162555,-0.254319232363049,
0.939198248544428));
#8684=CARTESIAN_POINT('Ctrl Pts',(0.564362943424238,-0.28018331644634,0.916597376014514));
#8685=CARTESIAN_POINT('Ctrl Pts',(0.585840553788742,-0.29104845371857,0.903141581680914));
#8686=CARTESIAN_POINT('Ctrl Pts',(0.629305439856167,-0.30527573347708,0.873412008702649));
#8687=CARTESIAN_POINT('Ctrl Pts',(0.651278921914856,-0.308638795020976,
0.857118508332695));
#8688=CARTESIAN_POINT('Ctrl Pts',(0.690705563850638,-0.308638795020976,
0.825676810575914));
#8689=CARTESIAN_POINT('Ctrl Pts',(0.711480111898423,-0.30527573347708,0.807879894508811));
#8690=CARTESIAN_POINT('Ctrl Pts',(0.750136149454208,-0.29104845371857,0.772120216227122));
#8691=CARTESIAN_POINT('Ctrl Pts',(0.768033796848072,-0.28018331644634,0.754175290318038));
#8692=CARTESIAN_POINT('Ctrl Pts',(0.798619410861634,-0.254319232363049,
0.721738358858166));
#8693=CARTESIAN_POINT('Ctrl Pts',(0.812805334167529,-0.237895043532788,
0.705614819529209));
#8694=CARTESIAN_POINT('Ctrl Pts',(0.837310877969633,-0.199697230012983,
0.676354402927683));
#8695=CARTESIAN_POINT('Ctrl Pts',(0.847641868610495,-0.177924977804098,
0.663225258065736));
#8696=CARTESIAN_POINT('Ctrl Pts',(0.866144010579847,-0.124911173756694,
0.638954437806245));
#8697=CARTESIAN_POINT('Ctrl Pts',(0.873158080166742,-0.0925528133349865,
0.62914037979579));
#8698=CARTESIAN_POINT('Ctrl Pts',(0.876916659919095,-0.05953,0.623857181492959));
#8699=CARTESIAN_POINT('',(0.437601487681057,-0.05953,1.03511272300331));
#8700=CARTESIAN_POINT('Origin',(0.685838782044607,-0.05953,0.860014630714833));
#8701=CARTESIAN_POINT('',(0.911784794170997,-0.05953,0.656964154625313));
#8702=CARTESIAN_POINT('Ctrl Pts',(0.911784794170998,-0.0595300000000001,
0.656964154625312));
#8703=CARTESIAN_POINT('Ctrl Pts',(0.909827729890942,-0.0762225747374255,
0.659680317203144));
#8704=CARTESIAN_POINT('Ctrl Pts',(0.907004864562642,-0.0928409665394228,
0.663576540841106));
#8705=CARTESIAN_POINT('Ctrl Pts',(0.895234408667242,-0.144299303100741,
0.679480524217551));
#8706=CARTESIAN_POINT('Ctrl Pts',(0.882797231409153,-0.177024326825049,
0.695831250979106));
#8707=CARTESIAN_POINT('Ctrl Pts',(0.854332839576145,-0.227269801620064,
0.73042219438957));
#8708=CARTESIAN_POINT('Ctrl Pts',(0.834863020612702,-0.251265615809407,
0.752807465209441));
#8709=CARTESIAN_POINT('Ctrl Pts',(0.800439809856111,-0.279889827963178,
0.789147407129766));
#8710=CARTESIAN_POINT('Ctrl Pts',(0.781998747691871,-0.290879136862659,
0.80756613568454));
#8711=CARTESIAN_POINT('Ctrl Pts',(0.742239891936898,-0.305251990234487,
0.844254137480382));
#8712=CARTESIAN_POINT('Ctrl Pts',(0.720906778729541,-0.308638795020976,
0.862505527716294));
#8713=CARTESIAN_POINT('Ctrl Pts',(0.680463863683392,-0.308638795020976,
0.894757676234429));
#8714=CARTESIAN_POINT('Ctrl Pts',(0.657923009631182,-0.305251990234488,
0.91149460735272));
#8715=CARTESIAN_POINT('Ctrl Pts',(0.613307674922609,-0.290879136862659,
0.942092777160053));
#8716=CARTESIAN_POINT('Ctrl Pts',(0.591247219971725,-0.279889827963178,
0.955972930713954));
#8717=CARTESIAN_POINT('Ctrl Pts',(0.548158511259202,-0.251265615809407,
0.981446681891443));
#8718=CARTESIAN_POINT('Ctrl Pts',(0.522002043615455,-0.227269801620063,
0.995447160474328));
#8719=CARTESIAN_POINT('Ctrl Pts',(0.481944444320713,-0.177024326825049,
1.01550068154148));
#8720=CARTESIAN_POINT('Ctrl Pts',(0.463236132117164,-0.14429930310074,1.0239876538093));
#8721=CARTESIAN_POINT('Ctrl Pts',(0.445111721969657,-0.0928409665394226,
1.03192403056628));
#8722=CARTESIAN_POINT('Ctrl Pts',(0.440685038163619,-0.0762225747374254,
1.03380912944435));
#8723=CARTESIAN_POINT('Ctrl Pts',(0.437601487681056,-0.05953,1.03511272300331));
#8724=CARTESIAN_POINT('Origin',(0.685838782044607,-0.05953,0.860014630714833));
#8725=CARTESIAN_POINT('Origin',(0.,-0.208355,0.));
#8726=CARTESIAN_POINT('',(0.0548532617164168,-0.05953,1.12247250791415));
#8727=CARTESIAN_POINT('Origin',(0.,-0.05953,0.));
#8728=CARTESIAN_POINT('',(-0.536443649899848,-0.05953,0.987512846410683));
#8729=CARTESIAN_POINT('Ctrl Pts',(0.0548532617164173,-0.0595300000000001,
1.12247250791414));
#8730=CARTESIAN_POINT('Ctrl Pts',(0.05150947068137,-0.0762225747374254,
1.12263591311425));
#8731=CARTESIAN_POINT('Ctrl Pts',(0.0467032526342597,-0.0928409665394227,
1.12285816383385));
#8732=CARTESIAN_POINT('Ctrl Pts',(0.0269302585198975,-0.144299303100741,
1.12357162229597));
#8733=CARTESIAN_POINT('Ctrl Pts',(0.006392292392153,-0.177024326825049,
1.12404235695137));
#8734=CARTESIAN_POINT('Ctrl Pts',(-0.0383992541984087,-0.227269801620063,
1.12335509974011));
#8735=CARTESIAN_POINT('Ctrl Pts',(-0.0680399972366993,-0.251265615809407,
1.12208997038458));
#8736=CARTESIAN_POINT('Ctrl Pts',(-0.117914228755037,-0.279889827963178,
1.1178344036749));
#8737=CARTESIAN_POINT('Ctrl Pts',(-0.14381238480104,-0.290879136862659,
1.11490049012186));
#8738=CARTESIAN_POINT('Ctrl Pts',(-0.19728546073067,-0.305251990234488,
1.10669035995599));
#8739=CARTESIAN_POINT('Ctrl Pts',(-0.224855950742601,-0.308638795020976,
1.10139101611326));
#8740=CARTESIAN_POINT('Ctrl Pts',(-0.275287440920027,-0.308638795020976,
1.0898803575765));
#8741=CARTESIAN_POINT('Ctrl Pts',(-0.302426893214945,-0.305251990234488,
1.08269251410343));
#8742=CARTESIAN_POINT('Ctrl Pts',(-0.35416671187353,-0.290879136862659,
1.06688848765783));
#8743=CARTESIAN_POINT('Ctrl Pts',(-0.3787731215897,-0.279889827963178,1.05829506364875));
#8744=CARTESIAN_POINT('Ctrl Pts',(-0.425554672694338,-0.251265615809407,
1.04048957871266));
#8745=CARTESIAN_POINT('Ctrl Pts',(-0.452808978448581,-0.227269801620063,
1.02876878445619));
#8746=CARTESIAN_POINT('Ctrl Pts',(-0.493462957200432,-0.177024326825049,
1.0099536580922));
#8747=CARTESIAN_POINT('Ctrl Pts',(-0.511762781179148,-0.14429930310074,
1.00061845128527));
#8748=CARTESIAN_POINT('Ctrl Pts',(-0.529268075276157,-0.0928409665394226,
0.991396466802468));
#8749=CARTESIAN_POINT('Ctrl Pts',(-0.533501897135713,-0.0762225747374254,
0.989110885965947));
#8750=CARTESIAN_POINT('Ctrl Pts',(-0.536443649899848,-0.0595300000000001,
0.987512846410683));
#8751=CARTESIAN_POINT('',(-0.843383895613249,-0.05953,0.742736168477219));
#8752=CARTESIAN_POINT('Origin',(0.,-0.05953,0.));
#8753=CARTESIAN_POINT('',(-1.10653577764992,-0.05953,0.196295654879792));
#8754=CARTESIAN_POINT('Ctrl Pts',(-0.843383895613249,-0.0595300000000001,
0.742736168477219));
#8755=CARTESIAN_POINT('Ctrl Pts',(-0.84559647055299,-0.0762225747374255,
0.740223768851062));
#8756=CARTESIAN_POINT('Ctrl Pts',(-0.848766861100456,-0.0928409665394227,
0.736604687327351));
#8757=CARTESIAN_POINT('Ctrl Pts',(-0.861652925570091,-0.144299303100741,
0.721590372101268));
#8758=CARTESIAN_POINT('Ctrl Pts',(-0.87482617317514,-0.177024326825049,
0.705826641853758));
#8759=CARTESIAN_POINT('Ctrl Pts',(-0.902215926359523,-0.227269801620063,
0.670378702718353));
#8760=CARTESIAN_POINT('Ctrl Pts',(-0.919707509403859,-0.251265615809407,
0.646415841396062));
#8761=CARTESIAN_POINT('Ctrl Pts',(-0.947476448101718,-0.279889827963178,
0.604769294586516));
#8762=CARTESIAN_POINT('Ctrl Pts',(-0.961329858300736,-0.290879136862659,
0.582692035672022));
#8763=CARTESIAN_POINT('Ctrl Pts',(-0.988250837578047,-0.305251990234488,
0.535766169015486));
#8764=CARTESIAN_POINT('Ctrl Pts',(-1.00129756308006,-0.308638795020976,
0.510906605094603));
#8765=CARTESIAN_POINT('Ctrl Pts',(-1.02374168767024,-0.308638795020976,
0.46430090015576));
#8766=CARTESIAN_POINT('Ctrl Pts',(-1.03504317708586,-0.305251990234488,
0.438600874831839));
#8767=CARTESIAN_POINT('Ctrl Pts',(-1.05494634094458,-0.290879136862659,
0.388295406390235));
#8768=CARTESIAN_POINT('Ctrl Pts',(-1.06356957703048,-0.279889827963178,
0.363699428370917));
#8769=CARTESIAN_POINT('Ctrl Pts',(-1.0788165083757,-0.251265615809407,0.316022600643821));
#8770=CARTESIAN_POINT('Ctrl Pts',(-1.08664560412098,-0.227269801620063,
0.287406530683752));
#8771=CARTESIAN_POINT('Ctrl Pts',(-1.09728268713976,-0.177024326825049,
0.243890930799337));
#8772=CARTESIAN_POINT('Ctrl Pts',(-1.10139388218929,-0.144299303100741,
0.22376314604679));
#8773=CARTESIAN_POINT('Ctrl Pts',(-1.10509821673782,-0.0928409665394227,
0.204327142733961));
#8774=CARTESIAN_POINT('Ctrl Pts',(-1.10595102243643,-0.0762225747374254,
0.199591971170104));
#8775=CARTESIAN_POINT('Ctrl Pts',(-1.10653577764992,-0.0595300000000001,
0.196295654879792));
#8776=CARTESIAN_POINT('',(-1.123812,-0.05953,1.37627276864339E-16));
#8777=CARTESIAN_POINT('Origin',(0.,-0.05953,0.));
#8778=CARTESIAN_POINT('',(-1.123812,-0.35718,1.37627276864339E-16));
#8779=CARTESIAN_POINT('',(-1.123812,-0.208355,1.37627276864339E-16));
#8780=CARTESIAN_POINT('Origin',(0.,-0.35718,0.));
#8781=CARTESIAN_POINT('',(-1.10653577764992,-0.05953,-0.196295654879793));
#8782=CARTESIAN_POINT('Origin',(0.,-0.05953,0.));
#8783=CARTESIAN_POINT('',(-0.843383895613249,-0.05953,-0.742736168477219));
#8784=CARTESIAN_POINT('Ctrl Pts',(-1.10653577764992,-0.0595300000000001,
-0.196295654879792));
#8785=CARTESIAN_POINT('Ctrl Pts',(-1.10595102243643,-0.0762225747374255,
-0.199591971170104));
#8786=CARTESIAN_POINT('Ctrl Pts',(-1.10509821673782,-0.0928409665394228,
-0.204327142733962));
#8787=CARTESIAN_POINT('Ctrl Pts',(-1.10139388218929,-0.144299303100741,
-0.22376314604679));
#8788=CARTESIAN_POINT('Ctrl Pts',(-1.09728268713976,-0.177024326825049,
-0.243890930799338));
#8789=CARTESIAN_POINT('Ctrl Pts',(-1.08664560412098,-0.227269801620063,
-0.287406530683753));
#8790=CARTESIAN_POINT('Ctrl Pts',(-1.0788165083757,-0.251265615809407,-0.316022600643821));
#8791=CARTESIAN_POINT('Ctrl Pts',(-1.06356957703048,-0.279889827963178,
-0.363699428370918));
#8792=CARTESIAN_POINT('Ctrl Pts',(-1.05494634094458,-0.290879136862659,
-0.388295406390235));
#8793=CARTESIAN_POINT('Ctrl Pts',(-1.03504317708586,-0.305251990234488,
-0.438600874831839));
#8794=CARTESIAN_POINT('Ctrl Pts',(-1.02374168767024,-0.308638795020976,
-0.46430090015576));
#8795=CARTESIAN_POINT('Ctrl Pts',(-1.00129756308006,-0.308638795020976,
-0.510906605094603));
#8796=CARTESIAN_POINT('Ctrl Pts',(-0.988250837578047,-0.305251990234488,
-0.535766169015486));
#8797=CARTESIAN_POINT('Ctrl Pts',(-0.961329858300736,-0.290879136862659,
-0.582692035672022));
#8798=CARTESIAN_POINT('Ctrl Pts',(-0.947476448101718,-0.279889827963178,
-0.604769294586516));
#8799=CARTESIAN_POINT('Ctrl Pts',(-0.919707509403859,-0.251265615809407,
-0.646415841396062));
#8800=CARTESIAN_POINT('Ctrl Pts',(-0.902215926359523,-0.227269801620064,
-0.670378702718353));
#8801=CARTESIAN_POINT('Ctrl Pts',(-0.87482617317514,-0.177024326825049,
-0.705826641853758));
#8802=CARTESIAN_POINT('Ctrl Pts',(-0.861652925570091,-0.144299303100741,
-0.721590372101268));
#8803=CARTESIAN_POINT('Ctrl Pts',(-0.848766861100456,-0.0928409665394229,
-0.736604687327351));
#8804=CARTESIAN_POINT('Ctrl Pts',(-0.84559647055299,-0.0762225747374255,
-0.740223768851063));
#8805=CARTESIAN_POINT('Ctrl Pts',(-0.843383895613249,-0.0595300000000001,
-0.742736168477219));
#8806=CARTESIAN_POINT('',(-0.536443649899847,-0.05953,-0.987512846410683));
#8807=CARTESIAN_POINT('Origin',(0.,-0.05953,0.));
#8808=CARTESIAN_POINT('',(0.0548532617164172,-0.05953,-1.12247250791415));
#8809=CARTESIAN_POINT('Ctrl Pts',(-0.536443649899848,-0.0595300000000001,
-0.987512846410683));
#8810=CARTESIAN_POINT('Ctrl Pts',(-0.533501897135712,-0.0762225747374254,
-0.989110885965947));
#8811=CARTESIAN_POINT('Ctrl Pts',(-0.529268075276156,-0.0928409665394227,
-0.991396466802469));
#8812=CARTESIAN_POINT('Ctrl Pts',(-0.511762781179147,-0.144299303100741,
-1.00061845128527));
#8813=CARTESIAN_POINT('Ctrl Pts',(-0.493462957200432,-0.177024326825049,
-1.0099536580922));
#8814=CARTESIAN_POINT('Ctrl Pts',(-0.45280897844858,-0.227269801620063,
-1.02876878445619));
#8815=CARTESIAN_POINT('Ctrl Pts',(-0.425554672694337,-0.251265615809407,
-1.04048957871266));
#8816=CARTESIAN_POINT('Ctrl Pts',(-0.3787731215897,-0.279889827963178,-1.05829506364875));
#8817=CARTESIAN_POINT('Ctrl Pts',(-0.354166711873529,-0.290879136862659,
-1.06688848765783));
#8818=CARTESIAN_POINT('Ctrl Pts',(-0.302426893214944,-0.305251990234488,
-1.08269251410343));
#8819=CARTESIAN_POINT('Ctrl Pts',(-0.275287440920027,-0.308638795020976,
-1.0898803575765));
#8820=CARTESIAN_POINT('Ctrl Pts',(-0.224855950742601,-0.308638795020976,
-1.10139101611326));
#8821=CARTESIAN_POINT('Ctrl Pts',(-0.19728546073067,-0.305251990234488,
-1.10669035995599));
#8822=CARTESIAN_POINT('Ctrl Pts',(-0.143812384801039,-0.290879136862659,
-1.11490049012186));
#8823=CARTESIAN_POINT('Ctrl Pts',(-0.117914228755037,-0.279889827963178,
-1.1178344036749));
#8824=CARTESIAN_POINT('Ctrl Pts',(-0.0680399972366989,-0.251265615809407,
-1.12208997038458));
#8825=CARTESIAN_POINT('Ctrl Pts',(-0.0383992541984084,-0.227269801620063,
-1.12335509974011));
#8826=CARTESIAN_POINT('Ctrl Pts',(0.00639229239215326,-0.177024326825049,
-1.12404235695137));
#8827=CARTESIAN_POINT('Ctrl Pts',(0.0269302585198977,-0.144299303100741,
-1.12357162229597));
#8828=CARTESIAN_POINT('Ctrl Pts',(0.04670325263426,-0.0928409665394228,
-1.12285816383385));
#8829=CARTESIAN_POINT('Ctrl Pts',(0.0515094706813703,-0.0762225747374255,
-1.12263591311425));
#8830=CARTESIAN_POINT('Ctrl Pts',(0.0548532617164176,-0.0595300000000001,
-1.12247250791414));
#8831=CARTESIAN_POINT('',(0.437601487681057,-0.05953,-1.03511272300331));
#8832=CARTESIAN_POINT('Origin',(0.,-0.05953,0.));
#8833=CARTESIAN_POINT('',(0.911784794170997,-0.05953,-0.656964154625313));
#8834=CARTESIAN_POINT('Ctrl Pts',(0.437601487681056,-0.0595300000000001,
-1.03511272300331));
#8835=CARTESIAN_POINT('Ctrl Pts',(0.440685038163619,-0.0762225747374255,
-1.03380912944435));
#8836=CARTESIAN_POINT('Ctrl Pts',(0.445111721969657,-0.0928409665394228,
-1.03192403056628));
#8837=CARTESIAN_POINT('Ctrl Pts',(0.463236132117164,-0.144299303100741,
-1.0239876538093));
#8838=CARTESIAN_POINT('Ctrl Pts',(0.481944444320713,-0.177024326825049,
-1.01550068154148));
#8839=CARTESIAN_POINT('Ctrl Pts',(0.522002043615455,-0.227269801620064,
-0.995447160474328));
#8840=CARTESIAN_POINT('Ctrl Pts',(0.548158511259203,-0.251265615809407,
-0.981446681891443));
#8841=CARTESIAN_POINT('Ctrl Pts',(0.591247219971725,-0.279889827963178,
-0.955972930713954));
#8842=CARTESIAN_POINT('Ctrl Pts',(0.613307674922609,-0.290879136862659,
-0.942092777160053));
#8843=CARTESIAN_POINT('Ctrl Pts',(0.657923009631182,-0.305251990234487,
-0.91149460735272));
#8844=CARTESIAN_POINT('Ctrl Pts',(0.680463863683393,-0.308638795020976,
-0.894757676234429));
#8845=CARTESIAN_POINT('Ctrl Pts',(0.720906778729542,-0.308638795020976,
-0.862505527716294));
#8846=CARTESIAN_POINT('Ctrl Pts',(0.742239891936899,-0.305251990234488,
-0.844254137480381));
#8847=CARTESIAN_POINT('Ctrl Pts',(0.781998747691872,-0.290879136862659,
-0.80756613568454));
#8848=CARTESIAN_POINT('Ctrl Pts',(0.800439809856112,-0.279889827963178,
-0.789147407129765));
#8849=CARTESIAN_POINT('Ctrl Pts',(0.834863020612702,-0.251265615809407,
-0.752807465209441));
#8850=CARTESIAN_POINT('Ctrl Pts',(0.854332839576145,-0.227269801620064,
-0.73042219438957));
#8851=CARTESIAN_POINT('Ctrl Pts',(0.882797231409153,-0.177024326825049,
-0.695831250979106));
#8852=CARTESIAN_POINT('Ctrl Pts',(0.895234408667242,-0.144299303100741,
-0.679480524217551));
#8853=CARTESIAN_POINT('Ctrl Pts',(0.907004864562642,-0.0928409665394228,
-0.663576540841106));
#8854=CARTESIAN_POINT('Ctrl Pts',(0.909827729890942,-0.0762225747374256,
-0.659680317203144));
#8855=CARTESIAN_POINT('Ctrl Pts',(0.911784794170998,-0.0595300000000001,
-0.656964154625312));
#8856=CARTESIAN_POINT('',(1.08212377959455,-0.05953,-0.303251606722892));
#8857=CARTESIAN_POINT('Origin',(0.,-0.05953,0.));
#8858=CARTESIAN_POINT('',(1.08212377959455,-0.05953,0.303251606722892));
#8859=CARTESIAN_POINT('Ctrl Pts',(1.08212377959455,-0.0595300000000001,
-0.303251606722892));
#8860=CARTESIAN_POINT('Ctrl Pts',(1.0830271513892,-0.0762225747374255,-0.300028012588062));
#8861=CARTESIAN_POINT('Ctrl Pts',(1.08431331394788,-0.0928409665394228,
-0.2953917518996));
#8862=CARTESIAN_POINT('Ctrl Pts',(1.08940878963422,-0.144299303100741,-0.276273267473431));
#8863=CARTESIAN_POINT('Ctrl Pts',(1.09443784939331,-0.177024326825049,-0.256354979351213));
#8864=CARTESIAN_POINT('Ctrl Pts',(1.10373487993589,-0.227269801620064,-0.212533521233765));
#8865=CARTESIAN_POINT('Ctrl Pts',(1.10909715583869,-0.251265615809407,-0.183354415742157));
#8866=CARTESIAN_POINT('Ctrl Pts',(1.1160463456491,-0.279889827963178,-0.133783682657561));
#8867=CARTESIAN_POINT('Ctrl Pts',(1.11894887330541,-0.290879136862659,-0.107881990270302));
#8868=CARTESIAN_POINT('Ctrl Pts',(1.12284346704144,-0.305251990234488,-0.0539226701638766));
#8869=CARTESIAN_POINT('Ctrl Pts',(1.123812,-0.308638795020976,-0.025864214957475));
#8870=CARTESIAN_POINT('Ctrl Pts',(1.123812,-0.308638795020976,0.025864214957475));
#8871=CARTESIAN_POINT('Ctrl Pts',(1.12284346704144,-0.305251990234488,0.0539226701638766));
#8872=CARTESIAN_POINT('Ctrl Pts',(1.11894887330541,-0.290879136862659,0.107881990270302));
#8873=CARTESIAN_POINT('Ctrl Pts',(1.1160463456491,-0.279889827963178,0.133783682657561));
#8874=CARTESIAN_POINT('Ctrl Pts',(1.10909715583869,-0.251265615809407,0.183354415742157));
#8875=CARTESIAN_POINT('Ctrl Pts',(1.10373487993589,-0.227269801620064,0.212533521233765));
#8876=CARTESIAN_POINT('Ctrl Pts',(1.09443784939331,-0.177024326825049,0.256354979351213));
#8877=CARTESIAN_POINT('Ctrl Pts',(1.08940878963422,-0.144299303100741,0.276273267473431));
#8878=CARTESIAN_POINT('Ctrl Pts',(1.08431331394788,-0.0928409665394228,
0.2953917518996));
#8879=CARTESIAN_POINT('Ctrl Pts',(1.0830271513892,-0.0762225747374255,0.300028012588062));
#8880=CARTESIAN_POINT('Ctrl Pts',(1.08212377959455,-0.0595300000000001,
0.303251606722892));
#8881=CARTESIAN_POINT('Origin',(0.,-0.05953,0.));
#8882=CARTESIAN_POINT('Origin',(0.,-0.05953,0.));
#8883=CARTESIAN_POINT('',(0.0589974094846122,-0.05953,1.07456964270265));
#8884=CARTESIAN_POINT('Origin',(0.,-0.05953,0.));
#8885=CARTESIAN_POINT('Origin',(-0.244773027351946,-0.05953,1.07242070340001));
#8886=CARTESIAN_POINT('Origin',(-0.244773027351946,0.,1.07242070340001));
#8887=CARTESIAN_POINT('',(-0.519393123750572,-0.05953,0.942555777842682));
#8888=CARTESIAN_POINT('Ctrl Pts',(-0.519393123750572,-0.05953,0.942555777842682));
#8889=CARTESIAN_POINT('Ctrl Pts',(-0.513714466572041,-0.0925528133349865,
0.945684988399766));
#8890=CARTESIAN_POINT('Ctrl Pts',(-0.503136848051455,-0.124911173756694,
0.951483858396181));
#8891=CARTESIAN_POINT('Ctrl Pts',(-0.47593627990192,-0.177924977804098,
0.965323333309091));
#8892=CARTESIAN_POINT('Ctrl Pts',(-0.460931856495794,-0.199697230012983,
0.972669835243841));
#8893=CARTESIAN_POINT('Ctrl Pts',(-0.426157505475872,-0.237895043532788,
0.988400002689705));
#8894=CARTESIAN_POINT('Ctrl Pts',(-0.406380688682952,-0.254319232363049,
0.996771768218699));
#8895=CARTESIAN_POINT('Ctrl Pts',(-0.364750145543744,-0.28018331644634,
1.01272583306292));
#8896=CARTESIAN_POINT('Ctrl Pts',(-0.340838910881557,-0.29104845371857,
1.02112815447116));
#8897=CARTESIAN_POINT('Ctrl Pts',(-0.290495481564827,-0.30527573347708,
1.036574285215));
#8898=CARTESIAN_POINT('Ctrl Pts',(-0.264056468041074,-0.308638795020976,
1.04359501395068));
#8899=CARTESIAN_POINT('Ctrl Pts',(-0.214892249704082,-0.308638795020976,
1.05481642595959));
#8900=CARTESIAN_POINT('Ctrl Pts',(-0.188025341585962,-0.30527573347708,
1.05996242598502));
#8901=CARTESIAN_POINT('Ctrl Pts',(-0.135965654106109,-0.29104845371857,
1.06788913840721));
#8902=CARTESIAN_POINT('Ctrl Pts',(-0.110776745452494,-0.28018331644634,
1.07069360430242));
#8903=CARTESIAN_POINT('Ctrl Pts',(-0.0663467128214646,-0.254319232363049,
1.07438230428002));
#8904=CARTESIAN_POINT('Ctrl Pts',(-0.0448960436540983,-0.237895043532788,
1.07542044338697));
#8905=CARTESIAN_POINT('Ctrl Pts',(-0.00674037211528124,-0.199697230012983,
1.07633607767727));
#8906=CARTESIAN_POINT('Ctrl Pts',(0.00996567398334777,-0.177924977804098,
1.07622728347683));
#8907=CARTESIAN_POINT('Ctrl Pts',(0.0404772621979741,-0.124911173756694,
1.07556023164702));
#8908=CARTESIAN_POINT('Ctrl Pts',(0.0525234025782719,-0.0925528133349865,
1.07492508698591));
#8909=CARTESIAN_POINT('Ctrl Pts',(0.0589974094846124,-0.05953,1.07456964270265));
#8910=CARTESIAN_POINT('Origin',(-0.244773027351946,-0.05953,1.07242070340001));
#8911=CARTESIAN_POINT('Origin',(0.,-0.05953,0.));
#8912=CARTESIAN_POINT('',(-0.803348093619616,-0.05953,0.716109245731214));
#8913=CARTESIAN_POINT('Origin',(0.,-0.05953,0.));
#8914=CARTESIAN_POINT('Origin',(-0.991065754692661,-0.05953,0.477272113029314));
#8915=CARTESIAN_POINT('Origin',(-0.991065754692661,0.,0.477272113029314));
#8916=CARTESIAN_POINT('',(-1.06075609691358,-0.05953,0.181596019242328));
#8917=CARTESIAN_POINT('Ctrl Pts',(-1.06075609691358,-0.05953,0.181596019242328));
#8918=CARTESIAN_POINT('Ctrl Pts',(-1.05966202740332,-0.0925528133349865,
0.187986803072856));
#8919=CARTESIAN_POINT('Ctrl Pts',(-1.05760072925372,-0.124911173756694,
0.199872254546857));
#8920=CARTESIAN_POINT('Ctrl Pts',(-1.05146158959546,-0.177924977804098,
0.22976728653846));
#8921=CARTESIAN_POINT('Ctrl Pts',(-1.04785021111757,-0.199697230012983,
0.246078686169301));
#8922=CARTESIAN_POINT('Ctrl Pts',(-1.03846709802406,-0.237895043532788,
0.283073967563097));
#8923=CARTESIAN_POINT('Ctrl Pts',(-1.03268176429485,-0.254319232363049,
0.303755815985685));
#8924=CARTESIAN_POINT('Ctrl Pts',(-1.01919893537026,-0.28018331644634,0.346251081972725));
#8925=CARTESIAN_POINT('Ctrl Pts',(-1.01085972381132,-0.29104845371857,0.370184399726282));
#8926=CARTESIAN_POINT('Ctrl Pts',(-0.99154738033959,-0.30527573347708,0.419174982698463));
#8927=CARTESIAN_POINT('Ctrl Pts',(-0.980551951791748,-0.308638795020976,
0.444223188605045));
#8928=CARTESIAN_POINT('Ctrl Pts',(-0.958671816228589,-0.308638795020976,
0.489657758261848));
#8929=CARTESIAN_POINT('Ctrl Pts',(-0.945943877838127,-0.30527573347708,
0.51387163140139));
#8930=CARTESIAN_POINT('Ctrl Pts',(-0.91968254693063,-0.29104845371857,0.559515758398093));
#8931=CARTESIAN_POINT('Ctrl Pts',(-0.906170138993533,-0.28018331644634,
0.580957796077825));
#8932=CARTESIAN_POINT('Ctrl Pts',(-0.8813524085237,-0.254319232363049,0.617994461173994));
#8933=CARTESIAN_POINT('Ctrl Pts',(-0.868789784891799,-0.237895043532788,
0.635412538795143));
#8934=CARTESIAN_POINT('Ctrl Pts',(-0.845715984518854,-0.199697230012983,
0.66581473268113));
#8935=CARTESIAN_POINT('Ctrl Pts',(-0.835214876415962,-0.177924977804098,
0.678808213394124));
#8936=CARTESIAN_POINT('Ctrl Pts',(-0.815669690204649,-0.124911173756694,
0.702247233627224));
#8937=CARTESIAN_POINT('Ctrl Pts',(-0.807662468433796,-0.0925528133349865,
0.711269279199861));
#8938=CARTESIAN_POINT('Ctrl Pts',(-0.803348093619616,-0.05953,0.716109245731214));
#8939=CARTESIAN_POINT('Origin',(-0.991065754692661,-0.05953,0.477272113029314));
#8940=CARTESIAN_POINT('Origin',(0.,-0.05953,0.));
#8941=CARTESIAN_POINT('',(-1.076188,-0.05953,1.31795018948079E-16));
#8942=CARTESIAN_POINT('Origin',(0.,-0.05953,0.));
#8943=CARTESIAN_POINT('',(-1.06075609691358,-0.05953,-0.181596019242328));
#8944=CARTESIAN_POINT('Origin',(0.,-0.05953,0.));
#8945=CARTESIAN_POINT('Origin',(-0.991065754692661,-0.05953,-0.477272113029314));
#8946=CARTESIAN_POINT('Origin',(-0.991065754692661,0.,-0.477272113029314));
#8947=CARTESIAN_POINT('',(-0.803348093619616,-0.05953,-0.716109245731215));
#8948=CARTESIAN_POINT('Ctrl Pts',(-0.803348093619616,-0.05953,-0.716109245731215));
#8949=CARTESIAN_POINT('Ctrl Pts',(-0.807662468433795,-0.0925528133349865,
-0.711269279199862));
#8950=CARTESIAN_POINT('Ctrl Pts',(-0.815669690204649,-0.124911173756694,
-0.702247233627224));
#8951=CARTESIAN_POINT('Ctrl Pts',(-0.835214876415962,-0.177924977804098,
-0.678808213394124));
#8952=CARTESIAN_POINT('Ctrl Pts',(-0.845715984518854,-0.199697230012983,
-0.66581473268113));
#8953=CARTESIAN_POINT('Ctrl Pts',(-0.868789784891799,-0.237895043532788,
-0.635412538795143));
#8954=CARTESIAN_POINT('Ctrl Pts',(-0.8813524085237,-0.254319232363049,-0.617994461173994));
#8955=CARTESIAN_POINT('Ctrl Pts',(-0.906170138993533,-0.28018331644634,
-0.580957796077826));
#8956=CARTESIAN_POINT('Ctrl Pts',(-0.91968254693063,-0.29104845371857,-0.559515758398093));
#8957=CARTESIAN_POINT('Ctrl Pts',(-0.945943877838127,-0.30527573347708,
-0.51387163140139));
#8958=CARTESIAN_POINT('Ctrl Pts',(-0.958671816228589,-0.308638795020976,
-0.489657758261848));
#8959=CARTESIAN_POINT('Ctrl Pts',(-0.980551951791748,-0.308638795020976,
-0.444223188605045));
#8960=CARTESIAN_POINT('Ctrl Pts',(-0.99154738033959,-0.30527573347708,-0.419174982698463));
#8961=CARTESIAN_POINT('Ctrl Pts',(-1.01085972381132,-0.29104845371857,-0.370184399726282));
#8962=CARTESIAN_POINT('Ctrl Pts',(-1.01919893537026,-0.28018331644634,-0.346251081972725));
#8963=CARTESIAN_POINT('Ctrl Pts',(-1.03268176429485,-0.254319232363049,
-0.303755815985685));
#8964=CARTESIAN_POINT('Ctrl Pts',(-1.03846709802406,-0.237895043532788,
-0.283073967563097));
#8965=CARTESIAN_POINT('Ctrl Pts',(-1.04785021111757,-0.199697230012983,
-0.246078686169302));
#8966=CARTESIAN_POINT('Ctrl Pts',(-1.05146158959546,-0.177924977804098,
-0.229767286538461));
#8967=CARTESIAN_POINT('Ctrl Pts',(-1.05760072925372,-0.124911173756694,
-0.199872254546858));
#8968=CARTESIAN_POINT('Ctrl Pts',(-1.05966202740332,-0.0925528133349864,
-0.187986803072857));
#8969=CARTESIAN_POINT('Ctrl Pts',(-1.06075609691358,-0.05953,-0.181596019242328));
#8970=CARTESIAN_POINT('Origin',(-0.991065754692661,-0.05953,-0.477272113029314));
#8971=CARTESIAN_POINT('Origin',(0.,-0.05953,0.));
#8972=CARTESIAN_POINT('',(-0.519393123750572,-0.05953,-0.942555777842682));
#8973=CARTESIAN_POINT('Origin',(0.,-0.05953,0.));
#8974=CARTESIAN_POINT('Origin',(-0.244773027351946,-0.05953,-1.07242070340001));
#8975=CARTESIAN_POINT('Origin',(-0.244773027351946,0.,-1.07242070340001));
#8976=CARTESIAN_POINT('',(0.0589974094846125,-0.05953,-1.07456964270265));
#8977=CARTESIAN_POINT('Ctrl Pts',(0.0589974094846127,-0.05953,-1.07456964270265));
#8978=CARTESIAN_POINT('Ctrl Pts',(0.0525234025782722,-0.0925528133349865,
-1.07492508698591));
#8979=CARTESIAN_POINT('Ctrl Pts',(0.0404772621979744,-0.124911173756694,
-1.07556023164702));
#8980=CARTESIAN_POINT('Ctrl Pts',(0.0099656739833481,-0.177924977804098,
-1.07622728347683));
#8981=CARTESIAN_POINT('Ctrl Pts',(-0.00674037211528096,-0.199697230012983,
-1.07633607767727));
#8982=CARTESIAN_POINT('Ctrl Pts',(-0.044896043654098,-0.237895043532788,
-1.07542044338697));
#8983=CARTESIAN_POINT('Ctrl Pts',(-0.0663467128214644,-0.254319232363049,
-1.07438230428002));
#8984=CARTESIAN_POINT('Ctrl Pts',(-0.110776745452493,-0.28018331644634,
-1.07069360430242));
#8985=CARTESIAN_POINT('Ctrl Pts',(-0.135965654106109,-0.29104845371857,
-1.06788913840721));
#8986=CARTESIAN_POINT('Ctrl Pts',(-0.188025341585962,-0.30527573347708,
-1.05996242598502));
#8987=CARTESIAN_POINT('Ctrl Pts',(-0.214892249704082,-0.308638795020976,
-1.05481642595959));
#8988=CARTESIAN_POINT('Ctrl Pts',(-0.264056468041074,-0.308638795020976,
-1.04359501395068));
#8989=CARTESIAN_POINT('Ctrl Pts',(-0.290495481564827,-0.30527573347708,
-1.036574285215));
#8990=CARTESIAN_POINT('Ctrl Pts',(-0.340838910881557,-0.291048453718569,
-1.02112815447116));
#8991=CARTESIAN_POINT('Ctrl Pts',(-0.364750145543744,-0.28018331644634,
-1.01272583306292));
#8992=CARTESIAN_POINT('Ctrl Pts',(-0.406380688682952,-0.254319232363049,
-0.996771768218699));
#8993=CARTESIAN_POINT('Ctrl Pts',(-0.426157505475872,-0.237895043532788,
-0.988400002689705));
#8994=CARTESIAN_POINT('Ctrl Pts',(-0.460931856495794,-0.199697230012983,
-0.972669835243841));
#8995=CARTESIAN_POINT('Ctrl Pts',(-0.475936279901919,-0.177924977804098,
-0.965323333309091));
#8996=CARTESIAN_POINT('Ctrl Pts',(-0.503136848051454,-0.124911173756694,
-0.951483858396181));
#8997=CARTESIAN_POINT('Ctrl Pts',(-0.513714466572041,-0.0925528133349865,
-0.945684988399766));
#8998=CARTESIAN_POINT('Ctrl Pts',(-0.519393123750572,-0.05953,-0.942555777842682));
#8999=CARTESIAN_POINT('Origin',(-0.244773027351946,-0.05953,-1.07242070340001));
#9000=CARTESIAN_POINT('Origin',(0.,-0.05953,0.));
#9001=CARTESIAN_POINT('',(0.413083465285518,-0.05953,-0.993751811093549));
#9002=CARTESIAN_POINT('Origin',(0.,-0.05953,0.));
#9003=CARTESIAN_POINT('Origin',(0.685838782044607,-0.05953,-0.860014630714833));
#9004=CARTESIAN_POINT('Origin',(0.685838782044607,0.,-0.860014630714833));
#9005=CARTESIAN_POINT('',(0.876916659919095,-0.05953,-0.623857181492959));
#9006=CARTESIAN_POINT('Ctrl Pts',(0.876916659919095,-0.05953,-0.623857181492958));
#9007=CARTESIAN_POINT('Ctrl Pts',(0.873158080166742,-0.0925528133349865,
-0.62914037979579));
#9008=CARTESIAN_POINT('Ctrl Pts',(0.866144010579847,-0.124911173756694,
-0.638954437806245));
#9009=CARTESIAN_POINT('Ctrl Pts',(0.847641868610495,-0.177924977804098,
-0.663225258065736));
#9010=CARTESIAN_POINT('Ctrl Pts',(0.837310877969633,-0.199697230012983,
-0.676354402927683));
#9011=CARTESIAN_POINT('Ctrl Pts',(0.81280533416753,-0.237895043532788,-0.705614819529209));
#9012=CARTESIAN_POINT('Ctrl Pts',(0.798619410861634,-0.254319232363049,
-0.721738358858166));
#9013=CARTESIAN_POINT('Ctrl Pts',(0.768033796848072,-0.28018331644634,-0.754175290318038));
#9014=CARTESIAN_POINT('Ctrl Pts',(0.750136149454208,-0.29104845371857,-0.772120216227122));
#9015=CARTESIAN_POINT('Ctrl Pts',(0.711480111898423,-0.30527573347708,-0.807879894508811));
#9016=CARTESIAN_POINT('Ctrl Pts',(0.690705563850638,-0.308638795020976,
-0.825676810575913));
#9017=CARTESIAN_POINT('Ctrl Pts',(0.651278921914856,-0.308638795020976,
-0.857118508332695));
#9018=CARTESIAN_POINT('Ctrl Pts',(0.629305439856167,-0.30527573347708,-0.873412008702649));
#9019=CARTESIAN_POINT('Ctrl Pts',(0.585840553788742,-0.29104845371857,-0.903141581680914));
#9020=CARTESIAN_POINT('Ctrl Pts',(0.564362943424239,-0.28018331644634,-0.916597376014514));
#9021=CARTESIAN_POINT('Ctrl Pts',(0.525933334162556,-0.254319232363049,
-0.939198248544427));
#9022=CARTESIAN_POINT('Ctrl Pts',(0.507057380724533,-0.237895043532788,
-0.949440676105255));
#9023=CARTESIAN_POINT('Ctrl Pts',(0.473077587363686,-0.199697230012983,
-0.966820759530997));
#9024=CARTESIAN_POINT('Ctrl Pts',(0.457978755888596,-0.177924977804098,
-0.973971221090534));
#9025=CARTESIAN_POINT('Ctrl Pts',(0.430199341854858,-0.124911173756694,
-0.986608710139579));
#9026=CARTESIAN_POINT('Ctrl Pts',(0.419070565453384,-0.0925528133349865,
-0.991263089003441));
#9027=CARTESIAN_POINT('Ctrl Pts',(0.413083465285518,-0.05953,-0.993751811093549));
#9028=CARTESIAN_POINT('Origin',(0.685838782044607,-0.05953,-0.860014630714833));
#9029=CARTESIAN_POINT('Origin',(0.,-0.208355,0.));
#9030=CARTESIAN_POINT('',(-1.076188,-0.35718,1.31795018948079E-16));
#9031=CARTESIAN_POINT('Origin',(0.,-0.35718,0.));
#9032=CARTESIAN_POINT('',(-1.076188,-0.208355,1.31795018948079E-16));
#9033=CARTESIAN_POINT('',(1.03449977959455,-0.05953,0.296632461748266));
#9034=CARTESIAN_POINT('Origin',(0.,-0.05953,0.));
#9035=CARTESIAN_POINT('',(1.03449977959455,-0.05953,-0.296632461748266));
#9036=CARTESIAN_POINT('Ctrl Pts',(1.03449977959455,-0.05953,0.296632461748267));
#9037=CARTESIAN_POINT('Ctrl Pts',(1.03628691421076,-0.0925528133349865,
0.290399865505497));
#9038=CARTESIAN_POINT('Ctrl Pts',(1.03958665287714,-0.124911173756694,0.278797079997872));
#9039=CARTESIAN_POINT('Ctrl Pts',(1.0470264474309,-0.177924977804098,0.249198913998601));
#9040=CARTESIAN_POINT('Ctrl Pts',(1.05084995891418,-0.199697230012983,0.232935932341942));
#9041=CARTESIAN_POINT('Ctrl Pts',(1.05844771715377,-0.237895043532788,0.195533155353269));
#9042=CARTESIAN_POINT('Ctrl Pts',(1.06220882929878,-0.254319232363049,0.17438929156337));
#9043=CARTESIAN_POINT('Ctrl Pts',(1.06849922508772,-0.28018331644634,0.130252399648131));
#9044=CARTESIAN_POINT('Ctrl Pts',(1.07137013248666,-0.29104845371857,0.105070977154072));
#9045=CARTESIAN_POINT('Ctrl Pts',(1.07522652957392,-0.30527573347708,0.0525526752791107));
#9046=CARTESIAN_POINT('Ctrl Pts',(1.076188,-0.308638795020976,0.025214283908933));
#9047=CARTESIAN_POINT('Ctrl Pts',(1.076188,-0.308638795020976,-0.025214283908933));
#9048=CARTESIAN_POINT('Ctrl Pts',(1.07522652957392,-0.30527573347708,-0.0525526752791107));
#9049=CARTESIAN_POINT('Ctrl Pts',(1.07137013248666,-0.29104845371857,-0.105070977154072));
#9050=CARTESIAN_POINT('Ctrl Pts',(1.06849922508772,-0.28018331644634,-0.130252399648131));
#9051=CARTESIAN_POINT('Ctrl Pts',(1.06220882929878,-0.254319232363049,-0.17438929156337));
#9052=CARTESIAN_POINT('Ctrl Pts',(1.05844771715377,-0.237895043532788,-0.195533155353269));
#9053=CARTESIAN_POINT('Ctrl Pts',(1.05084995891418,-0.199697230012983,-0.232935932341942));
#9054=CARTESIAN_POINT('Ctrl Pts',(1.0470264474309,-0.177924977804098,-0.249198913998601));
#9055=CARTESIAN_POINT('Ctrl Pts',(1.03958665287714,-0.124911173756694,-0.278797079997872));
#9056=CARTESIAN_POINT('Ctrl Pts',(1.03628691421076,-0.0925528133349865,
-0.290399865505497));
#9057=CARTESIAN_POINT('Ctrl Pts',(1.03449977959455,-0.05953,-0.296632461748267));
#9058=CARTESIAN_POINT('Origin',(0.,-0.05953,0.));
#9059=CARTESIAN_POINT('Origin',(0.,-0.05953,0.));
#9060=CARTESIAN_POINT('Origin',(1.1,-0.05953,0.));
#9061=CARTESIAN_POINT('Origin',(1.1,0.,0.));
#9062=CARTESIAN_POINT('Origin',(1.1,-0.05953,0.));
#9063=CARTESIAN_POINT('Origin',(0.,-0.35718,0.));
#9064=CARTESIAN_POINT('Origin',(0.,-0.05953,0.));
#9065=CARTESIAN_POINT('',(0.,0.,0.));
#9066=CARTESIAN_POINT('Origin',(1.119765,0.495,0.));
#9067=CARTESIAN_POINT('',(-1.119765,0.495,-1.37131662304724E-16));
#9068=CARTESIAN_POINT('Origin',(0.,0.495,0.));
#9069=CARTESIAN_POINT('',(-1.085235,0.495,-1.32902956907268E-16));
#9070=CARTESIAN_POINT('Origin',(0.,0.495,0.));
#9071=CARTESIAN_POINT('Origin',(0.,0.4575,0.));
#9072=CARTESIAN_POINT('',(-1.119765,0.42,-1.37131662304724E-16));
#9073=CARTESIAN_POINT('Origin',(0.,0.42,0.));
#9074=CARTESIAN_POINT('',(-1.119765,0.4575,-1.37131662304724E-16));
#9075=CARTESIAN_POINT('Origin',(1.085235,0.42,0.));
#9076=CARTESIAN_POINT('',(-1.085235,0.42,-1.32902956907268E-16));
#9077=CARTESIAN_POINT('Origin',(0.,0.42,0.));
#9078=CARTESIAN_POINT('Origin',(0.,0.4575,0.));
#9079=CARTESIAN_POINT('',(-1.085235,0.4575,-1.32902956907268E-16));
#9080=CARTESIAN_POINT('Origin',(1.119765,-0.42,0.));
#9081=CARTESIAN_POINT('',(-1.119765,-0.42,-1.37131662304724E-16));
#9082=CARTESIAN_POINT('Origin',(0.,-0.42,0.));
#9083=CARTESIAN_POINT('',(-1.085235,-0.42,-1.32902956907268E-16));
#9084=CARTESIAN_POINT('Origin',(0.,-0.42,0.));
#9085=CARTESIAN_POINT('Origin',(0.,-0.4575,0.));
#9086=CARTESIAN_POINT('',(-1.119765,-0.495,-1.37131662304724E-16));
#9087=CARTESIAN_POINT('Origin',(0.,-0.495,0.));
#9088=CARTESIAN_POINT('',(-1.119765,-0.4575,-1.37131662304724E-16));
#9089=CARTESIAN_POINT('Origin',(1.085235,-0.495,0.));
#9090=CARTESIAN_POINT('',(-1.085235,-0.495,-1.32902956907268E-16));
#9091=CARTESIAN_POINT('Origin',(0.,-0.495,0.));
#9092=CARTESIAN_POINT('Origin',(0.,-0.4575,0.));
#9093=CARTESIAN_POINT('',(-1.085235,-0.4575,-1.32902956907268E-16));
#9094=CARTESIAN_POINT('',(0.,0.,0.));
#9095=CARTESIAN_POINT('',(0.,0.,0.));
#9096=CARTESIAN_POINT('',(0.,0.,0.));
#9097=CARTESIAN_POINT('',(0.,0.,0.));
#9098=CARTESIAN_POINT('',(0.,0.,0.));
#9099=CARTESIAN_POINT('',(0.,0.,0.));
#9100=CARTESIAN_POINT('',(0.,0.,0.));
#9101=CARTESIAN_POINT('Origin',(-0.2,-3.5,9.3));
#9102=CARTESIAN_POINT('',(-0.2,-1.5,9.43431457505076));
#9103=CARTESIAN_POINT('',(-0.2,-3.5,9.43431457505076));
#9104=CARTESIAN_POINT('',(-0.2,-4.,9.43431457505076));
#9105=CARTESIAN_POINT('',(-0.2,-1.5,9.65));
#9106=CARTESIAN_POINT('',(-0.2,-1.5,9.65));
#9107=CARTESIAN_POINT('',(-0.2,-3.5,9.65));
#9108=CARTESIAN_POINT('',(-0.2,-3.5,9.65));
#9109=CARTESIAN_POINT('',(-0.2,-3.5,9.65));
#9110=CARTESIAN_POINT('Origin',(0.,-3.5,9.475));
#9111=CARTESIAN_POINT('',(0.2,-3.5,9.43431457505076));
#9112=CARTESIAN_POINT('Origin',(0.,-3.5,10.));
#9113=CARTESIAN_POINT('',(0.2,-3.5,9.65));
#9114=CARTESIAN_POINT('',(0.2,-3.5,9.65));
#9115=CARTESIAN_POINT('',(0.2,-3.5,9.3));
#9116=CARTESIAN_POINT('Origin',(0.2,-3.5,9.65));
#9117=CARTESIAN_POINT('',(0.2,-1.5,9.43431457505076));
#9118=CARTESIAN_POINT('',(0.2,-4.,9.43431457505076));
#9119=CARTESIAN_POINT('',(0.2,-1.5,9.65));
#9120=CARTESIAN_POINT('',(0.2,-3.5,9.65));
#9121=CARTESIAN_POINT('',(0.2,-1.5,9.3));
#9122=CARTESIAN_POINT('Origin',(-0.2,-3.5,9.65));
#9123=CARTESIAN_POINT('',(0.2,-1.5,9.65));
#9124=CARTESIAN_POINT('Origin',(0.,-1.5,9.475));
#9125=CARTESIAN_POINT('Origin',(0.,-1.5,10.));
#9126=CARTESIAN_POINT('Origin',(0.,-0.5,10.));
#9127=CARTESIAN_POINT('',(-0.8,-0.5,10.));
#9128=CARTESIAN_POINT('Origin',(0.,-0.5,10.));
#9129=CARTESIAN_POINT('',(-0.6,-0.5,10.));
#9130=CARTESIAN_POINT('Origin',(0.,-0.5,10.));
#9131=CARTESIAN_POINT('Origin',(0.,-0.8,10.));
#9132=CARTESIAN_POINT('',(-0.8,-0.8,10.));
#9133=CARTESIAN_POINT('Origin',(0.,-0.8,10.));
#9134=CARTESIAN_POINT('',(-0.6,-0.8,10.));
#9135=CARTESIAN_POINT('Origin',(0.,-0.8,10.));
#9136=CARTESIAN_POINT('Origin',(0.,-0.8,10.));
#9137=CARTESIAN_POINT('',(-0.8,-0.8,10.));
#9138=CARTESIAN_POINT('Origin',(0.,-4.,10.));
#9139=CARTESIAN_POINT('',(-0.6,-4.,10.));
#9140=CARTESIAN_POINT('',(-0.6,-4.,10.));
#9141=CARTESIAN_POINT('Origin',(0.,-4.,10.));
#9142=CARTESIAN_POINT('Origin',(0.,-4.,10.));
#9143=CARTESIAN_POINT('',(-0.6,6.,10.));
#9144=CARTESIAN_POINT('Origin',(0.,6.,10.));
#9145=CARTESIAN_POINT('',(-0.6,-4.,10.));
#9146=CARTESIAN_POINT('Origin',(0.,6.,10.));
#9147=CARTESIAN_POINT('Origin',(0.,-4.,10.));
#9148=CARTESIAN_POINT('',(0.,0.,0.));
#9149=CARTESIAN_POINT('Origin',(5.3,-3.1,10.));
#9150=CARTESIAN_POINT('',(5.135,-3.,10.));
#9151=CARTESIAN_POINT('Origin',(5.3,-3.,10.));
#9152=CARTESIAN_POINT('',(5.135,-2.2,10.));
#9153=CARTESIAN_POINT('',(5.135,-3.1,10.));
#9154=CARTESIAN_POINT('Origin',(5.3,-2.2,10.));
#9155=CARTESIAN_POINT('Origin',(7.7,-3.1,10.));
#9156=CARTESIAN_POINT('',(7.535,-3.,10.));
#9157=CARTESIAN_POINT('Origin',(7.7,-3.,10.));
#9158=CARTESIAN_POINT('',(7.535,-2.2,10.));
#9159=CARTESIAN_POINT('',(7.535,-3.1,10.));
#9160=CARTESIAN_POINT('Origin',(7.7,-2.2,10.));
#9161=CARTESIAN_POINT('Origin',(0.,-2.,10.59));
#9162=CARTESIAN_POINT('',(0.109087121146348,-2.17944358444927,10.59));
#9163=CARTESIAN_POINT('',(0.109087121146348,-1.82055641555073,10.59));
#9164=CARTESIAN_POINT('',(0.109087121146348,-3.5,10.59));
#9165=CARTESIAN_POINT('Origin',(0.,-2.,10.59));
#9166=CARTESIAN_POINT('Origin',(0.,-2.,10.59));
#9167=CARTESIAN_POINT('',(-0.109087121146348,-2.17944358444927,10.59));
#9168=CARTESIAN_POINT('Ctrl Pts',(-0.109087121146349,-2.17944358444927,
10.59));
#9169=CARTESIAN_POINT('Ctrl Pts',(-0.100058962329428,-2.18493197155217,
10.5916692472112));
#9170=CARTESIAN_POINT('Ctrl Pts',(-0.0905297208284635,-2.18978489888129,
10.5932143633855));
#9171=CARTESIAN_POINT('Ctrl Pts',(-0.0548356965671432,-2.20463697075952,
10.598057680137));
#9172=CARTESIAN_POINT('Ctrl Pts',(-0.0266060994851221,-2.21,10.6));
#9173=CARTESIAN_POINT('Ctrl Pts',(0.026606099485122,-2.21,10.6));
#9174=CARTESIAN_POINT('Ctrl Pts',(0.0548356965671431,-2.20463697075952,
10.598057680137));
#9175=CARTESIAN_POINT('Ctrl Pts',(0.0905297208284635,-2.18978489888129,
10.5932143633855));
#9176=CARTESIAN_POINT('Ctrl Pts',(0.100058962329428,-2.18493197155217,10.5916692472112));
#9177=CARTESIAN_POINT('Ctrl Pts',(0.109087121146348,-2.17944358444927,10.59));
#9178=CARTESIAN_POINT('',(-0.21,-2.,10.59));
#9179=CARTESIAN_POINT('Origin',(0.,-2.,10.59));
#9180=CARTESIAN_POINT('',(-0.21,-2.,11.4852272553384));
#9181=CARTESIAN_POINT('',(-0.21,-2.,10.59));
#9182=CARTESIAN_POINT('',(0.21,-2.,11.4852272553384));
#9183=CARTESIAN_POINT('Ctrl Pts',(0.21,-2.,11.4852272553384));
#9184=CARTESIAN_POINT('Ctrl Pts',(0.21,-2.02640552692445,11.4852272553384));
#9185=CARTESIAN_POINT('Ctrl Pts',(0.204715737269596,-2.05454707409071,11.4860041595441));
#9186=CARTESIAN_POINT('Ctrl Pts',(0.183273763036332,-2.10627626890513,11.4888007328232));
#9187=CARTESIAN_POINT('Ctrl Pts',(0.167117923970394,-2.12986692412796,11.4907789715758));
#9188=CARTESIAN_POINT('Ctrl Pts',(0.129867169887369,-2.16711767821098,11.4944848114133));
#9189=CARTESIAN_POINT('Ctrl Pts',(0.106276408305765,-2.18327371000135,11.4964545565713));
#9190=CARTESIAN_POINT('Ctrl Pts',(0.0545468514059001,-2.20471582482622,
11.4992316551565));
#9191=CARTESIAN_POINT('Ctrl Pts',(0.0264051785092814,-2.21,11.5));
#9192=CARTESIAN_POINT('Ctrl Pts',(-0.0264051785092814,-2.21,11.5));
#9193=CARTESIAN_POINT('Ctrl Pts',(-0.0545468514059001,-2.20471582482622,
11.4992316551565));
#9194=CARTESIAN_POINT('Ctrl Pts',(-0.106276408305765,-2.18327371000135,
11.4964545565713));
#9195=CARTESIAN_POINT('Ctrl Pts',(-0.129867169887369,-2.16711767821098,
11.4944848114133));
#9196=CARTESIAN_POINT('Ctrl Pts',(-0.167117923970394,-2.12986692412796,
11.4907789715758));
#9197=CARTESIAN_POINT('Ctrl Pts',(-0.183273763036332,-2.10627626890513,
11.4888007328232));
#9198=CARTESIAN_POINT('Ctrl Pts',(-0.204715737269596,-2.05454707409071,
11.4860041595441));
#9199=CARTESIAN_POINT('Ctrl Pts',(-0.21,-2.02640552692445,11.4852272553384));
#9200=CARTESIAN_POINT('Ctrl Pts',(-0.21,-2.,11.4852272553384));
#9201=CARTESIAN_POINT('Ctrl Pts',(-0.21,-2.,11.4852272553384));
#9202=CARTESIAN_POINT('Ctrl Pts',(-0.21,-1.97359447307555,11.4852272553384));
#9203=CARTESIAN_POINT('Ctrl Pts',(-0.204715737269596,-1.94545292590929,
11.4860041595441));
#9204=CARTESIAN_POINT('Ctrl Pts',(-0.183273763036331,-1.89372373109487,
11.4888007328232));
#9205=CARTESIAN_POINT('Ctrl Pts',(-0.167117923970394,-1.87013307587204,
11.4907789715758));
#9206=CARTESIAN_POINT('Ctrl Pts',(-0.129867169887369,-1.83288232178902,
11.4944848114133));
#9207=CARTESIAN_POINT('Ctrl Pts',(-0.106276408305765,-1.81672628999865,
11.4964545565713));
#9208=CARTESIAN_POINT('Ctrl Pts',(-0.0545468514059002,-1.79528417517378,
11.4992316551565));
#9209=CARTESIAN_POINT('Ctrl Pts',(-0.0264051785092814,-1.79,11.5));
#9210=CARTESIAN_POINT('Ctrl Pts',(0.0264051785092814,-1.79,11.5));
#9211=CARTESIAN_POINT('Ctrl Pts',(0.0545468514059001,-1.79528417517378,
11.4992316551565));
#9212=CARTESIAN_POINT('Ctrl Pts',(0.106276408305765,-1.81672628999865,11.4964545565713));
#9213=CARTESIAN_POINT('Ctrl Pts',(0.129867169887369,-1.83288232178902,11.4944848114133));
#9214=CARTESIAN_POINT('Ctrl Pts',(0.167117923970394,-1.87013307587204,11.4907789715758));
#9215=CARTESIAN_POINT('Ctrl Pts',(0.183273763036331,-1.89372373109487,11.4888007328232));
#9216=CARTESIAN_POINT('Ctrl Pts',(0.204715737269596,-1.94545292590929,11.4860041595441));
#9217=CARTESIAN_POINT('Ctrl Pts',(0.21,-1.97359447307555,11.4852272553384));
#9218=CARTESIAN_POINT('Ctrl Pts',(0.21,-2.,11.4852272553384));
#9219=CARTESIAN_POINT('',(-0.109087121146348,-1.82055641555073,10.59));
#9220=CARTESIAN_POINT('Origin',(0.,-2.,10.59));
#9221=CARTESIAN_POINT('Ctrl Pts',(0.109087121146348,-1.82055641555073,10.59));
#9222=CARTESIAN_POINT('Ctrl Pts',(0.100058962329427,-1.81506802844783,10.5916692472112));
#9223=CARTESIAN_POINT('Ctrl Pts',(0.0905297208284631,-1.81021510111871,
10.5932143633855));
#9224=CARTESIAN_POINT('Ctrl Pts',(0.054835696567143,-1.79536302924048,10.598057680137));
#9225=CARTESIAN_POINT('Ctrl Pts',(0.026606099485122,-1.79,10.6));
#9226=CARTESIAN_POINT('Ctrl Pts',(-0.026606099485122,-1.79,10.6));
#9227=CARTESIAN_POINT('Ctrl Pts',(-0.0548356965671429,-1.79536302924048,
10.598057680137));
#9228=CARTESIAN_POINT('Ctrl Pts',(-0.0905297208284631,-1.81021510111871,
10.5932143633855));
#9229=CARTESIAN_POINT('Ctrl Pts',(-0.100058962329428,-1.81506802844783,
10.5916692472112));
#9230=CARTESIAN_POINT('Ctrl Pts',(-0.109087121146348,-1.82055641555073,
10.59));
#9231=CARTESIAN_POINT('Origin',(0.,-2.,10.59));
#9232=CARTESIAN_POINT('',(-0.109087121146348,-3.5,10.59));
#9233=CARTESIAN_POINT('Origin',(-0.2,-3.6,9.22));
#9234=CARTESIAN_POINT('',(-0.2,-3.5,9.22));
#9235=CARTESIAN_POINT('',(-0.2,-3.5,9.43431457505076));
#9236=CARTESIAN_POINT('',(-0.2,-3.5,9.61));
#9237=CARTESIAN_POINT('',(-0.2,-1.5,9.22));
#9238=CARTESIAN_POINT('',(-0.2,-3.6,9.22));
#9239=CARTESIAN_POINT('',(-0.2,-1.5,9.43431457505076));
#9240=CARTESIAN_POINT('',(-0.2,-1.5,9.61));
#9241=CARTESIAN_POINT('',(-0.2,-3.5,9.43431457505076));
#9242=CARTESIAN_POINT('Origin',(0.2,-3.6,9.22));
#9243=CARTESIAN_POINT('',(0.2,-3.5,9.22));
#9244=CARTESIAN_POINT('',(0.1,-3.5,9.22));
#9245=CARTESIAN_POINT('',(0.2,-1.5,9.22));
#9246=CARTESIAN_POINT('',(0.2,-3.6,9.22));
#9247=CARTESIAN_POINT('',(0.1,-1.5,9.22));
#9248=CARTESIAN_POINT('Origin',(0.2,-3.6,10.));
#9249=CARTESIAN_POINT('',(0.2,-3.5,9.43431457505076));
#9250=CARTESIAN_POINT('',(0.2,-3.5,10.));
#9251=CARTESIAN_POINT('',(0.2,-1.5,9.43431457505076));
#9252=CARTESIAN_POINT('',(0.2,-3.5,9.43431457505076));
#9253=CARTESIAN_POINT('',(0.2,-1.5,10.));
#9254=CARTESIAN_POINT('Origin',(0.,-1.5,10.));
#9255=CARTESIAN_POINT('',(-1.5,-1.5,10.));
#9256=CARTESIAN_POINT('Origin',(0.,-1.5,10.));
#9257=CARTESIAN_POINT('Origin',(0.,-1.5,10.));
#9258=CARTESIAN_POINT('Origin',(0.,-3.5,10.));
#9259=CARTESIAN_POINT('Origin',(0.,-3.5,10.));
#9260=CARTESIAN_POINT('Origin',(-0.266987298107781,-3.,8.53756443470179));
#9261=CARTESIAN_POINT('',(-3.18335633348014,-2.2,3.48626509181623));
#9262=CARTESIAN_POINT('',(-3.18335633348014,-3.,3.48626509181623));
#9263=CARTESIAN_POINT('',(-3.18335633348014,-3.,3.48626509181623));
#9264=CARTESIAN_POINT('',(-0.27409407929433,-2.2,8.52525512860841));
#9265=CARTESIAN_POINT('',(-3.26698729810778,-2.2,3.34141201199516));
#9266=CARTESIAN_POINT('',(-0.27409407929433,-3.,8.52525512860841));
#9267=CARTESIAN_POINT('',(-0.274094079294329,-3.5,8.52525512860841));
#9268=CARTESIAN_POINT('',(-3.26698729810778,-3.,3.34141201199516));
#9269=CARTESIAN_POINT('Origin',(-4.13301270189222,-3.,3.84141201199516));
#9270=CARTESIAN_POINT('',(-4.04938173726458,-3.,3.98626509181623));
#9271=CARTESIAN_POINT('',(-4.04938173726458,-2.2,3.98626509181623));
#9272=CARTESIAN_POINT('',(-4.04938173726458,-3.,3.98626509181623));
#9273=CARTESIAN_POINT('',(-1.14011948307877,-3.,9.02525512860841));
#9274=CARTESIAN_POINT('',(-1.13301270189222,-3.,9.03756443470179));
#9275=CARTESIAN_POINT('',(-1.14011948307877,-2.2,9.02525512860841));
#9276=CARTESIAN_POINT('',(-1.14011948307877,-3.5,9.02525512860841));
#9277=CARTESIAN_POINT('',(-1.13301270189222,-2.2,9.03756443470179));
#9278=CARTESIAN_POINT('Origin',(0.,-3.,10.));
#9279=CARTESIAN_POINT('',(-8.,-3.,10.));
#9280=CARTESIAN_POINT('Origin',(0.,-3.,10.));
#9281=CARTESIAN_POINT('',(-4.04938173726458,-3.,16.0137349081838));
#9282=CARTESIAN_POINT('Origin',(0.,-3.,10.));
#9283=CARTESIAN_POINT('',(-1.14011948307877,-3.,10.9747448713916));
#9284=CARTESIAN_POINT('',(-4.13301270189222,-3.,16.1585879880048));
#9285=CARTESIAN_POINT('',(-0.274094079294328,-3.,11.4747448713916));
#9286=CARTESIAN_POINT('Origin',(0.,-3.,10.));
#9287=CARTESIAN_POINT('',(-3.18335633348014,-3.,16.5137349081838));
#9288=CARTESIAN_POINT('',(-0.26698729810778,-3.,11.4624355652982));
#9289=CARTESIAN_POINT('',(7.23273807074472,-3.,10.5));
#9290=CARTESIAN_POINT('Origin',(0.,-3.,10.));
#9291=CARTESIAN_POINT('',(1.4142135623731,-3.,10.5));
#9292=CARTESIAN_POINT('',(7.4,-3.,10.5));
#9293=CARTESIAN_POINT('',(1.4142135623731,-3.,9.5));
#9294=CARTESIAN_POINT('Origin',(0.,-3.,10.));
#9295=CARTESIAN_POINT('',(7.23273807074472,-3.,9.5));
#9296=CARTESIAN_POINT('',(1.4,-3.,9.5));
#9297=CARTESIAN_POINT('Origin',(0.,-3.,10.));
#9298=CARTESIAN_POINT('Origin',(0.,-3.,10.));
#9299=CARTESIAN_POINT('Origin',(0.,-3.,10.));
#9300=CARTESIAN_POINT('',(-4.04938173726458,-2.2,16.0137349081838));
#9301=CARTESIAN_POINT('Origin',(0.,-2.2,10.));
#9302=CARTESIAN_POINT('',(-4.04938173726458,-3.,16.0137349081838));
#9303=CARTESIAN_POINT('Origin',(-1.13301270189222,-3.,10.9624355652982));
#9304=CARTESIAN_POINT('',(-1.14011948307877,-2.2,10.9747448713916));
#9305=CARTESIAN_POINT('',(-4.13301270189222,-2.2,16.1585879880048));
#9306=CARTESIAN_POINT('',(-1.14011948307877,-3.5,10.9747448713916));
#9307=CARTESIAN_POINT('Origin',(-3.26698729810778,-3.,16.6585879880048));
#9308=CARTESIAN_POINT('',(-3.18335633348014,-2.2,16.5137349081838));
#9309=CARTESIAN_POINT('',(-3.18335633348014,-3.,16.5137349081838));
#9310=CARTESIAN_POINT('',(-0.274094079294328,-2.2,11.4747448713916));
#9311=CARTESIAN_POINT('',(-0.274094079294328,-3.5,11.4747448713916));
#9312=CARTESIAN_POINT('',(-0.26698729810778,-2.2,11.4624355652982));
#9313=CARTESIAN_POINT('Origin',(0.,-3.,10.));
#9314=CARTESIAN_POINT('',(7.23273807074472,-2.2,10.5));
#9315=CARTESIAN_POINT('Origin',(0.,-2.2,10.));
#9316=CARTESIAN_POINT('',(7.23273807074472,-3.,10.5));
#9317=CARTESIAN_POINT('Origin',(1.4,-3.,10.5));
#9318=CARTESIAN_POINT('',(1.4142135623731,-2.2,10.5));
#9319=CARTESIAN_POINT('',(1.4142135623731,-3.5,10.5));
#9320=CARTESIAN_POINT('',(7.4,-2.2,10.5));
#9321=CARTESIAN_POINT('Origin',(7.4,-3.,9.5));
#9322=CARTESIAN_POINT('',(1.4142135623731,-2.2,9.5));
#9323=CARTESIAN_POINT('',(1.4142135623731,-3.5,9.5));
#9324=CARTESIAN_POINT('',(7.23273807074472,-2.2,9.5));
#9325=CARTESIAN_POINT('',(1.4,-2.2,9.5));
#9326=CARTESIAN_POINT('',(7.23273807074472,-3.,9.5));
#9327=CARTESIAN_POINT('Origin',(0.,-2.2,10.));
#9328=CARTESIAN_POINT('',(-8.,-2.2,10.));
#9329=CARTESIAN_POINT('Origin',(0.,-2.2,10.));
#9330=CARTESIAN_POINT('Origin',(0.,-2.2,10.));
#9331=CARTESIAN_POINT('Origin',(0.,-2.2,10.));
#9332=CARTESIAN_POINT('Origin',(0.,-2.2,10.));
#9333=CARTESIAN_POINT('Origin',(0.,-2.2,10.));
#9334=CARTESIAN_POINT('Origin',(0.,-3.,10.));
#9335=CARTESIAN_POINT('Origin',(0.,-3.,10.));
#9336=CARTESIAN_POINT('',(-8.,-3.,10.));
#9337=CARTESIAN_POINT('Origin',(0.,-3.5,10.));
#9338=CARTESIAN_POINT('',(-1.5,-3.5,10.));
#9339=CARTESIAN_POINT('',(-1.5,-3.5,10.));
#9340=CARTESIAN_POINT('Origin',(0.,-3.5,10.));
#9341=CARTESIAN_POINT('Origin',(0.,-3.5,10.));
#9342=CARTESIAN_POINT('',(0.,0.,0.));
#9343=CARTESIAN_POINT('Origin',(0.,4.5,10.));
#9344=CARTESIAN_POINT('',(-0.605,4.9,10.));
#9345=CARTESIAN_POINT('Origin',(0.,4.9,10.));
#9346=CARTESIAN_POINT('',(-0.605,4.5,10.));
#9347=CARTESIAN_POINT('',(-0.605,4.5,10.));
#9348=CARTESIAN_POINT('Origin',(0.,4.5,10.));
#9349=CARTESIAN_POINT('Origin',(0.,4.5,10.));
#9350=CARTESIAN_POINT('',(-0.8,4.9,10.));
#9351=CARTESIAN_POINT('Origin',(0.,4.9,10.));
#9352=CARTESIAN_POINT('',(-0.8,4.5,10.));
#9353=CARTESIAN_POINT('',(-0.8,4.5,10.));
#9354=CARTESIAN_POINT('Origin',(0.,4.5,10.));
#9355=CARTESIAN_POINT('Origin',(0.,4.9,10.));
#9356=CARTESIAN_POINT('Origin',(0.,4.5,10.));
#9357=CARTESIAN_POINT('',(0.,0.,0.));
#9358=CARTESIAN_POINT('Origin',(0.,5.3,10.59));
#9359=CARTESIAN_POINT('',(0.133884278389952,5.13821310312636,10.59));
#9360=CARTESIAN_POINT('',(0.133884278389952,5.46178689687364,10.59));
#9361=CARTESIAN_POINT('',(0.133884278389952,4.9,10.59));
#9362=CARTESIAN_POINT('Origin',(0.,5.3,10.59));
#9363=CARTESIAN_POINT('Origin',(0.,5.3,10.59));
#9364=CARTESIAN_POINT('',(-0.133884278389952,5.13821310312636,10.59));
#9365=CARTESIAN_POINT('Ctrl Pts',(-0.133884278389952,5.13821310312636,10.59));
#9366=CARTESIAN_POINT('Ctrl Pts',(-0.118254395260799,5.12527883178237,10.5935467722442));
#9367=CARTESIAN_POINT('Ctrl Pts',(-0.100109787682297,5.11420068341256,10.5969822478996));
#9368=CARTESIAN_POINT('Ctrl Pts',(-0.0548298721325188,5.09536143894557,
10.6030741628997));
#9369=CARTESIAN_POINT('Ctrl Pts',(-0.0266020595922903,5.09,10.605));
#9370=CARTESIAN_POINT('Ctrl Pts',(0.0266020595922903,5.09,10.605));
#9371=CARTESIAN_POINT('Ctrl Pts',(0.0548298721325188,5.09536143894557,10.6030741628997));
#9372=CARTESIAN_POINT('Ctrl Pts',(0.100109787682297,5.11420068341256,10.5969822478996));
#9373=CARTESIAN_POINT('Ctrl Pts',(0.118254395260799,5.12527883178237,10.5935467722442));
#9374=CARTESIAN_POINT('Ctrl Pts',(0.133884278389952,5.13821310312636,10.59));
#9375=CARTESIAN_POINT('',(-0.21,5.3,10.59));
#9376=CARTESIAN_POINT('Origin',(0.,5.3,10.59));
#9377=CARTESIAN_POINT('',(-0.21,5.3,11.0797684937059));
#9378=CARTESIAN_POINT('',(-0.21,5.3,10.59));
#9379=CARTESIAN_POINT('',(0.21,5.3,11.0797684937059));
#9380=CARTESIAN_POINT('Ctrl Pts',(0.21,5.3,11.0797684937059));
#9381=CARTESIAN_POINT('Ctrl Pts',(0.21,5.27356141186949,11.0797684937059));
#9382=CARTESIAN_POINT('Ctrl Pts',(0.204702922670976,5.24540621874507,11.0808401566467));
#9383=CARTESIAN_POINT('Ctrl Pts',(0.183251796806354,5.19368655445866,11.0846831370713));
#9384=CARTESIAN_POINT('Ctrl Pts',(0.167101177357215,5.17011632925886,11.0873959305462));
#9385=CARTESIAN_POINT('Ctrl Pts',(0.129884533480965,5.13289968538261,11.0924663328912));
#9386=CARTESIAN_POINT('Ctrl Pts',(0.106313940757289,5.11674838983659,11.0951573889536));
#9387=CARTESIAN_POINT('Ctrl Pts',(0.0545930033295207,5.09529677343026,11.0989503922059));
#9388=CARTESIAN_POINT('Ctrl Pts',(0.0264373623835353,5.09,11.1));
#9389=CARTESIAN_POINT('Ctrl Pts',(-0.0264373623835352,5.09,11.1));
#9390=CARTESIAN_POINT('Ctrl Pts',(-0.0545930033295207,5.09529677343026,
11.0989503922059));
#9391=CARTESIAN_POINT('Ctrl Pts',(-0.106313940757289,5.11674838983659,11.0951573889536));
#9392=CARTESIAN_POINT('Ctrl Pts',(-0.129884533480965,5.13289968538261,11.0924663328912));
#9393=CARTESIAN_POINT('Ctrl Pts',(-0.167101177357215,5.17011632925886,11.0873959305462));
#9394=CARTESIAN_POINT('Ctrl Pts',(-0.183251796806354,5.19368655445866,11.0846831370713));
#9395=CARTESIAN_POINT('Ctrl Pts',(-0.204702922670976,5.24540621874507,11.0808401566467));
#9396=CARTESIAN_POINT('Ctrl Pts',(-0.21,5.27356141186949,11.0797684937059));
#9397=CARTESIAN_POINT('Ctrl Pts',(-0.21,5.3,11.0797684937059));
#9398=CARTESIAN_POINT('Ctrl Pts',(-0.21,5.3,11.0797684937059));
#9399=CARTESIAN_POINT('Ctrl Pts',(-0.21,5.32643858813051,11.0797684937059));
#9400=CARTESIAN_POINT('Ctrl Pts',(-0.204702922670976,5.35459378125493,11.0808401566467));
#9401=CARTESIAN_POINT('Ctrl Pts',(-0.183251796806354,5.40631344554134,11.0846831370713));
#9402=CARTESIAN_POINT('Ctrl Pts',(-0.167101177357215,5.42988367074114,11.0873959305462));
#9403=CARTESIAN_POINT('Ctrl Pts',(-0.129884533480965,5.46710031461738,11.0924663328912));
#9404=CARTESIAN_POINT('Ctrl Pts',(-0.106313940757289,5.48325161016341,11.0951573889536));
#9405=CARTESIAN_POINT('Ctrl Pts',(-0.0545930033295208,5.50470322656974,
11.0989503922059));
#9406=CARTESIAN_POINT('Ctrl Pts',(-0.0264373623835353,5.51,11.1));
#9407=CARTESIAN_POINT('Ctrl Pts',(0.0264373623835352,5.51,11.1));
#9408=CARTESIAN_POINT('Ctrl Pts',(0.0545930033295208,5.50470322656974,11.0989503922059));
#9409=CARTESIAN_POINT('Ctrl Pts',(0.106313940757289,5.48325161016341,11.0951573889536));
#9410=CARTESIAN_POINT('Ctrl Pts',(0.129884533480965,5.46710031461738,11.0924663328912));
#9411=CARTESIAN_POINT('Ctrl Pts',(0.167101177357214,5.42988367074114,11.0873959305462));
#9412=CARTESIAN_POINT('Ctrl Pts',(0.183251796806354,5.40631344554134,11.0846831370713));
#9413=CARTESIAN_POINT('Ctrl Pts',(0.204702922670976,5.35459378125493,11.0808401566467));
#9414=CARTESIAN_POINT('Ctrl Pts',(0.21,5.32643858813051,11.0797684937059));
#9415=CARTESIAN_POINT('Ctrl Pts',(0.21,5.3,11.0797684937059));
#9416=CARTESIAN_POINT('',(-0.133884278389952,5.46178689687364,10.59));
#9417=CARTESIAN_POINT('Origin',(0.,5.3,10.59));
#9418=CARTESIAN_POINT('Ctrl Pts',(0.133884278389952,5.46178689687364,10.59));
#9419=CARTESIAN_POINT('Ctrl Pts',(0.118254395260798,5.47472116821763,10.5935467722442));
#9420=CARTESIAN_POINT('Ctrl Pts',(0.100109787682297,5.48579931658744,10.5969822478996));
#9421=CARTESIAN_POINT('Ctrl Pts',(0.0548298721325188,5.50463856105443,10.6030741628997));
#9422=CARTESIAN_POINT('Ctrl Pts',(0.0266020595922903,5.51,10.605));
#9423=CARTESIAN_POINT('Ctrl Pts',(-0.0266020595922903,5.51,10.605));
#9424=CARTESIAN_POINT('Ctrl Pts',(-0.0548298721325188,5.50463856105443,
10.6030741628997));
#9425=CARTESIAN_POINT('Ctrl Pts',(-0.100109787682297,5.48579931658744,10.5969822478996));
#9426=CARTESIAN_POINT('Ctrl Pts',(-0.118254395260799,5.47472116821763,10.5935467722442));
#9427=CARTESIAN_POINT('Ctrl Pts',(-0.133884278389952,5.46178689687364,10.59));
#9428=CARTESIAN_POINT('Origin',(0.,5.3,10.59));
#9429=CARTESIAN_POINT('',(-0.133884278389952,4.9,10.59));
#9430=CARTESIAN_POINT('Origin',(0.,4.9,10.));
#9431=CARTESIAN_POINT('',(-0.605,5.7,10.));
#9432=CARTESIAN_POINT('Origin',(0.,5.7,10.));
#9433=CARTESIAN_POINT('',(-0.605,4.9,10.));
#9434=CARTESIAN_POINT('',(-0.605,4.9,10.));
#9435=CARTESIAN_POINT('Origin',(0.,4.9,10.));
#9436=CARTESIAN_POINT('Origin',(0.,4.9,10.));
#9437=CARTESIAN_POINT('',(-1.1,5.7,10.));
#9438=CARTESIAN_POINT('Origin',(0.,5.7,10.));
#9439=CARTESIAN_POINT('',(-1.1,4.9,10.));
#9440=CARTESIAN_POINT('',(-1.1,4.9,10.));
#9441=CARTESIAN_POINT('Origin',(0.,4.9,10.));
#9442=CARTESIAN_POINT('Origin',(0.,5.7,10.));
#9443=CARTESIAN_POINT('Origin',(0.,4.9,10.));
#9444=CARTESIAN_POINT('',(0.,0.,0.));
#9445=CARTESIAN_POINT('Origin',(6.5,-6.1,10.));
#9446=CARTESIAN_POINT('',(6.335,-6.,10.));
#9447=CARTESIAN_POINT('Origin',(6.5,-6.,10.));
#9448=CARTESIAN_POINT('',(6.335,-4.3,10.));
#9449=CARTESIAN_POINT('',(6.335,-6.1,10.));
#9450=CARTESIAN_POINT('Origin',(6.5,-4.3,10.));
#9451=CARTESIAN_POINT('Origin',(6.5,-4.3,10.));
#9452=CARTESIAN_POINT('Origin',(5.3,-3.5,10.));
#9453=CARTESIAN_POINT('',(5.075,-3.4,10.));
#9454=CARTESIAN_POINT('Origin',(5.3,-3.4,10.));
#9455=CARTESIAN_POINT('',(5.075,-3.,10.));
#9456=CARTESIAN_POINT('',(5.075,-3.5,10.));
#9457=CARTESIAN_POINT('Origin',(5.3,-3.,10.));
#9458=CARTESIAN_POINT('Origin',(7.7,-3.5,10.));
#9459=CARTESIAN_POINT('',(7.475,-3.4,10.));
#9460=CARTESIAN_POINT('Origin',(7.7,-3.4,10.));
#9461=CARTESIAN_POINT('',(7.475,-3.,10.));
#9462=CARTESIAN_POINT('',(7.475,-3.5,10.));
#9463=CARTESIAN_POINT('Origin',(7.7,-3.,10.));
#9464=CARTESIAN_POINT('Origin',(6.5,-3.4,10.));
#9465=CARTESIAN_POINT('',(4.8,-3.4,10.));
#9466=CARTESIAN_POINT('Origin',(6.5,-3.4,10.));
#9467=CARTESIAN_POINT('',(5.8,-3.4,10.));
#9468=CARTESIAN_POINT('Origin',(6.5,-3.4,10.));
#9469=CARTESIAN_POINT('Origin',(6.5,-3.4,10.));
#9470=CARTESIAN_POINT('',(4.8,-3.,10.));
#9471=CARTESIAN_POINT('Origin',(6.5,-3.,10.));
#9472=CARTESIAN_POINT('',(4.8,-3.4,10.));
#9473=CARTESIAN_POINT('Origin',(6.5,-4.55,10.));
#9474=CARTESIAN_POINT('',(5.8,-4.55,10.));
#9475=CARTESIAN_POINT('Origin',(6.5,-4.55,10.));
#9476=CARTESIAN_POINT('',(6.,-4.55,10.));
#9477=CARTESIAN_POINT('Origin',(6.5,-4.55,10.));
#9478=CARTESIAN_POINT('Origin',(6.5,-4.55,10.));
#9479=CARTESIAN_POINT('',(5.8,-4.55,10.));
#9480=CARTESIAN_POINT('Origin',(6.5,-6.,10.));
#9481=CARTESIAN_POINT('',(6.,-6.,10.));
#9482=CARTESIAN_POINT('',(6.,-6.,10.));
#9483=CARTESIAN_POINT('Origin',(6.5,-6.,10.));
#9484=CARTESIAN_POINT('Origin',(6.5,-3.,10.));
#9485=CARTESIAN_POINT('Origin',(6.5,-6.,10.));
#9486=CARTESIAN_POINT('',(0.,0.,0.));
#9487=CARTESIAN_POINT('Origin',(6.5,-6.,10.));
#9488=CARTESIAN_POINT('',(5.995,-5.45,10.));
#9489=CARTESIAN_POINT('Origin',(6.5,-5.45,10.));
#9490=CARTESIAN_POINT('',(5.995,-6.,10.));
#9491=CARTESIAN_POINT('',(5.995,-6.,10.));
#9492=CARTESIAN_POINT('Origin',(6.5,-6.,10.));
#9493=CARTESIAN_POINT('Origin',(6.5,-6.,10.));
#9494=CARTESIAN_POINT('',(5.8,-5.45,10.));
#9495=CARTESIAN_POINT('Origin',(6.5,-5.45,10.));
#9496=CARTESIAN_POINT('',(5.8,-6.,10.));
#9497=CARTESIAN_POINT('',(5.8,-6.,10.));
#9498=CARTESIAN_POINT('Origin',(6.5,-6.,10.));
#9499=CARTESIAN_POINT('Origin',(6.5,-5.45,10.));
#9500=CARTESIAN_POINT('Origin',(6.5,-6.,10.));
#9501=CARTESIAN_POINT('',(0.,0.,0.));
#9502=CARTESIAN_POINT('Origin',(6.5,-6.2,10.));
#9503=CARTESIAN_POINT('',(6.275,-6.,10.));
#9504=CARTESIAN_POINT('Origin',(6.5,-6.,10.));
#9505=CARTESIAN_POINT('',(6.275,-6.2,10.));
#9506=CARTESIAN_POINT('',(6.275,-6.2,10.));
#9507=CARTESIAN_POINT('Origin',(6.5,-6.2,10.));
#9508=CARTESIAN_POINT('Origin',(6.5,-6.2,10.));
#9509=CARTESIAN_POINT('',(5.6,-6.,10.));
#9510=CARTESIAN_POINT('Origin',(6.5,-6.,10.));
#9511=CARTESIAN_POINT('',(5.6,-6.2,10.));
#9512=CARTESIAN_POINT('',(5.6,-6.2,10.));
#9513=CARTESIAN_POINT('Origin',(6.5,-6.2,10.));
#9514=CARTESIAN_POINT('Origin',(6.5,-6.,10.));
#9515=CARTESIAN_POINT('Origin',(6.5,-6.2,10.));
#9516=CARTESIAN_POINT('',(0.,0.,0.));
#9517=CARTESIAN_POINT('Origin',(0.4,0.18,0.38));
#9518=CARTESIAN_POINT('',(-0.8,0.2,0.36));
#9519=CARTESIAN_POINT('',(-0.8,0.16,0.4));
#9520=CARTESIAN_POINT('',(-0.8,0.2,0.36));
#9521=CARTESIAN_POINT('',(0.8,0.16,0.4));
#9522=CARTESIAN_POINT('',(0.4,0.16,0.4));
#9523=CARTESIAN_POINT('',(0.8,0.2,0.36));
#9524=CARTESIAN_POINT('',(0.8,0.16,0.4));
#9525=CARTESIAN_POINT('',(0.4,0.2,0.36));
#9526=CARTESIAN_POINT('Origin',(-0.8,0.,0.38));
#9527=CARTESIAN_POINT('',(-0.8,-0.2,0.36));
#9528=CARTESIAN_POINT('',(-0.8,-0.16,0.4));
#9529=CARTESIAN_POINT('',(-0.8,-0.2,0.36));
#9530=CARTESIAN_POINT('Origin',(-0.8,0.,0.4));
#9531=CARTESIAN_POINT('Origin',(-0.8,0.,0.36));
#9532=CARTESIAN_POINT('Origin',(-0.4,-0.18,0.38));
#9533=CARTESIAN_POINT('',(0.8,-0.2,0.36));
#9534=CARTESIAN_POINT('',(0.8,-0.16,0.4));
#9535=CARTESIAN_POINT('',(0.8,-0.2,0.36));
#9536=CARTESIAN_POINT('',(-0.4,-0.16,0.4));
#9537=CARTESIAN_POINT('',(-0.4,-0.2,0.36));
#9538=CARTESIAN_POINT('Origin',(0.8,0.,0.38));
#9539=CARTESIAN_POINT('Origin',(0.8,0.,0.4));
#9540=CARTESIAN_POINT('Origin',(0.8,0.,0.36));
#9541=CARTESIAN_POINT('Origin',(-0.8,0.,0.));
#9542=CARTESIAN_POINT('',(-0.8,0.2,0.04));
#9543=CARTESIAN_POINT('',(-0.8,0.2,0.));
#9544=CARTESIAN_POINT('',(-0.8,-0.2,0.04));
#9545=CARTESIAN_POINT('Origin',(-0.8,0.,0.04));
#9546=CARTESIAN_POINT('',(-0.8,-0.2,0.));
#9547=CARTESIAN_POINT('Origin',(0.8,0.2,0.));
#9548=CARTESIAN_POINT('',(0.8,0.2,0.04));
#9549=CARTESIAN_POINT('',(0.8,0.2,0.));
#9550=CARTESIAN_POINT('',(0.4,0.2,0.04));
#9551=CARTESIAN_POINT('Origin',(0.,0.,0.4));
#9552=CARTESIAN_POINT('Origin',(0.4,0.18,0.02));
#9553=CARTESIAN_POINT('',(-0.8,0.16,0.));
#9554=CARTESIAN_POINT('',(-0.8,0.16,0.));
#9555=CARTESIAN_POINT('',(0.8,0.16,0.));
#9556=CARTESIAN_POINT('',(0.8,0.2,0.04));
#9557=CARTESIAN_POINT('',(0.4,0.16,0.));
#9558=CARTESIAN_POINT('Origin',(-0.8,0.,0.02));
#9559=CARTESIAN_POINT('',(-0.8,-0.16,0.));
#9560=CARTESIAN_POINT('',(-0.8,-0.16,0.));
#9561=CARTESIAN_POINT('Origin',(-0.8,0.,0.));
#9562=CARTESIAN_POINT('Origin',(-0.4,-0.18,0.02));
#9563=CARTESIAN_POINT('',(0.8,-0.16,0.));
#9564=CARTESIAN_POINT('',(0.8,-0.2,0.04));
#9565=CARTESIAN_POINT('',(0.8,-0.16,0.));
#9566=CARTESIAN_POINT('',(-0.4,-0.2,0.04));
#9567=CARTESIAN_POINT('',(-0.4,-0.16,0.));
#9568=CARTESIAN_POINT('Origin',(0.8,0.,0.02));
#9569=CARTESIAN_POINT('Origin',(0.8,0.,0.04));
#9570=CARTESIAN_POINT('Origin',(0.8,0.,0.));
#9571=CARTESIAN_POINT('Origin',(0.8,0.,0.));
#9572=CARTESIAN_POINT('',(0.8,-0.2,0.));
#9573=CARTESIAN_POINT('Origin',(0.,0.,0.));
#9574=CARTESIAN_POINT('Origin',(-0.8,-0.2,0.));
#9575=CARTESIAN_POINT('',(0.,0.,0.));
#9576=CARTESIAN_POINT('Origin',(0.0721687836487032,0.,-0.125));
#9577=CARTESIAN_POINT('',(0.0721687836487032,0.,-0.125));
#9578=CARTESIAN_POINT('',(0.144337567297406,0.,0.));
#9579=CARTESIAN_POINT('',(0.117710979560879,0.,-0.0461186027918559));
#9580=CARTESIAN_POINT('',(0.0721687836487032,-0.25,-0.125));
#9581=CARTESIAN_POINT('',(0.0721687836487032,0.,-0.125));
#9582=CARTESIAN_POINT('',(0.144337567297406,-0.25,0.));
#9583=CARTESIAN_POINT('',(0.144337567297406,-0.25,0.));
#9584=CARTESIAN_POINT('',(0.144337567297406,0.,0.));
#9585=CARTESIAN_POINT('Origin',(-0.0721687836487032,0.,-0.125));
#9586=CARTESIAN_POINT('',(-0.0721687836487032,0.,-0.125));
#9587=CARTESIAN_POINT('',(0.0739156081756484,0.,-0.125));
#9588=CARTESIAN_POINT('',(-0.0721687836487032,-0.25,-0.125));
#9589=CARTESIAN_POINT('',(-0.0721687836487032,0.,-0.125));
#9590=CARTESIAN_POINT('',(0.0721687836487032,-0.25,-0.125));
#9591=CARTESIAN_POINT('Origin',(-0.144337567297406,0.,-4.16333634234434E-17));
#9592=CARTESIAN_POINT('',(-0.144337567297406,0.,-1.76762539787485E-17));
#9593=CARTESIAN_POINT('',(-0.0987953713852306,0.,-0.0788813972081442));
#9594=CARTESIAN_POINT('',(-0.144337567297406,-0.25,-2.77555756156289E-17));
#9595=CARTESIAN_POINT('',(-0.144337567297406,0.,-1.76762539787485E-17));
#9596=CARTESIAN_POINT('',(-0.0721687836487032,-0.25,-0.125));
#9597=CARTESIAN_POINT('Origin',(-0.0721687836487033,0.,0.125));
#9598=CARTESIAN_POINT('',(-0.0721687836487033,0.,0.125));
#9599=CARTESIAN_POINT('',(-0.0627109795608791,0.,0.141381397208144));
#9600=CARTESIAN_POINT('',(-0.0721687836487033,-0.25,0.125));
#9601=CARTESIAN_POINT('',(-0.0721687836487033,0.,0.125));
#9602=CARTESIAN_POINT('',(-0.144337567297406,-0.25,-1.76762539787485E-17));
#9603=CARTESIAN_POINT('Origin',(0.0721687836487032,0.,0.125));
#9604=CARTESIAN_POINT('',(0.0721687836487032,0.,0.125));
#9605=CARTESIAN_POINT('',(0.146084391824352,0.,0.125));
#9606=CARTESIAN_POINT('',(0.0721687836487032,-0.25,0.125));
#9607=CARTESIAN_POINT('',(0.0721687836487032,0.,0.125));
#9608=CARTESIAN_POINT('',(-0.0721687836487033,-0.25,0.125));
#9609=CARTESIAN_POINT('Origin',(0.144337567297406,0.,0.));
#9610=CARTESIAN_POINT('',(0.153795371385231,0.,-0.0163813972081441));
#9611=CARTESIAN_POINT('',(0.0721687836487032,-0.25,0.125));
#9612=CARTESIAN_POINT('Origin',(0.,-0.25,0.));
#9613=CARTESIAN_POINT('Origin',(0.22,0.,0.));
#9614=CARTESIAN_POINT('',(-0.22,-8.67361737988404E-18,-2.69422295812418E-17));
#9615=CARTESIAN_POINT('Origin',(0.,0.,0.));
#9616=CARTESIAN_POINT('Origin',(0.,-0.015,0.));
#9617=CARTESIAN_POINT('',(-0.24505,-0.02505,-3.00099698131059E-17));
#9618=CARTESIAN_POINT('Origin',(0.,-0.02505,0.));
#9619=CARTESIAN_POINT('',(-0.235,-0.015,-2.87791997799628E-17));
#9620=CARTESIAN_POINT('Origin',(0.,-0.3775,0.));
#9621=CARTESIAN_POINT('',(-0.24505,-0.72995,3.00099698131059E-17));
#9622=CARTESIAN_POINT('Origin',(0.,-0.72995,0.));
#9623=CARTESIAN_POINT('',(-0.24505,-0.3775,-3.00099698131059E-17));
#9624=CARTESIAN_POINT('Origin',(0.,-0.7625,0.));
#9625=CARTESIAN_POINT('',(-0.175,-0.8,-2.14313189850787E-17));
#9626=CARTESIAN_POINT('Origin',(0.,-0.8,0.));
#9627=CARTESIAN_POINT('',(-0.2125,-0.7625,-2.60237444818813E-17));
#9628=CARTESIAN_POINT('Origin',(0.,-0.8,0.));
#9629=CARTESIAN_POINT('',(0.,0.,0.));
#9630=CARTESIAN_POINT('Origin',(0.0866025403784439,-0.4,-0.15));
#9631=CARTESIAN_POINT('',(0.173205080756888,-0.4,0.));
#9632=CARTESIAN_POINT('',(0.0866025403784439,-0.4,-0.15));
#9633=CARTESIAN_POINT('',(0.173205080756888,-0.4,0.));
#9634=CARTESIAN_POINT('',(0.0866025403784439,-0.64,-0.15));
#9635=CARTESIAN_POINT('',(0.0866025403784439,-0.4,-0.15));
#9636=CARTESIAN_POINT('',(0.173205080756888,-0.64,0.));
#9637=CARTESIAN_POINT('',(0.173205080756888,-0.64,0.));
#9638=CARTESIAN_POINT('',(0.173205080756888,-0.4,0.));
#9639=CARTESIAN_POINT('Origin',(-0.0866025403784438,-0.4,-0.15));
#9640=CARTESIAN_POINT('',(-0.0866025403784438,-0.4,-0.15));
#9641=CARTESIAN_POINT('',(0.0866025403784439,-0.4,-0.15));
#9642=CARTESIAN_POINT('',(-0.0866025403784438,-0.64,-0.15));
#9643=CARTESIAN_POINT('',(-0.0866025403784438,-0.4,-0.15));
#9644=CARTESIAN_POINT('',(0.0866025403784439,-0.64,-0.15));
#9645=CARTESIAN_POINT('Origin',(-0.173205080756888,-0.4,-2.77555756156289E-17));
#9646=CARTESIAN_POINT('',(-0.173205080756888,-0.4,-2.12115047744981E-17));
#9647=CARTESIAN_POINT('',(-0.0866025403784438,-0.4,-0.15));
#9648=CARTESIAN_POINT('',(-0.173205080756888,-0.64,-2.77555756156289E-17));
#9649=CARTESIAN_POINT('',(-0.173205080756888,-0.4,-2.12115047744981E-17));
#9650=CARTESIAN_POINT('',(-0.0866025403784438,-0.64,-0.15));
#9651=CARTESIAN_POINT('Origin',(-0.0866025403784439,-0.4,0.15));
#9652=CARTESIAN_POINT('',(-0.0866025403784439,-0.4,0.15));
#9653=CARTESIAN_POINT('',(-0.173205080756888,-0.4,-2.12115047744981E-17));
#9654=CARTESIAN_POINT('',(-0.0866025403784439,-0.64,0.15));
#9655=CARTESIAN_POINT('',(-0.0866025403784439,-0.4,0.15));
#9656=CARTESIAN_POINT('',(-0.173205080756888,-0.64,-2.12115047744981E-17));
#9657=CARTESIAN_POINT('Origin',(0.0866025403784439,-0.4,0.15));
#9658=CARTESIAN_POINT('',(0.0866025403784439,-0.4,0.15));
#9659=CARTESIAN_POINT('',(-0.0866025403784439,-0.4,0.15));
#9660=CARTESIAN_POINT('',(0.0866025403784439,-0.64,0.15));
#9661=CARTESIAN_POINT('',(0.0866025403784439,-0.4,0.15));
#9662=CARTESIAN_POINT('',(-0.0866025403784439,-0.64,0.15));
#9663=CARTESIAN_POINT('Origin',(0.173205080756888,-0.4,0.));
#9664=CARTESIAN_POINT('',(0.0866025403784439,-0.4,0.15));
#9665=CARTESIAN_POINT('',(0.0866025403784439,-0.64,0.15));
#9666=CARTESIAN_POINT('Origin',(0.,-0.4,-2.77555756156289E-17));
#9667=CARTESIAN_POINT('Origin',(0.,-0.64,-2.77555756156289E-17));
#9668=CARTESIAN_POINT('Origin',(0.,-1.,0.));
#9669=CARTESIAN_POINT('',(-0.1954,-1.,2.39295984553393E-17));
#9670=CARTESIAN_POINT('Origin',(0.,-1.,0.));
#9671=CARTESIAN_POINT('Origin',(0.3,0.4,0.));
#9672=CARTESIAN_POINT('',(-0.3,0.4,-3.67394039744206E-17));
#9673=CARTESIAN_POINT('Origin',(0.,0.4,0.));
#9674=CARTESIAN_POINT('Origin',(0.,0.375,0.));
#9675=CARTESIAN_POINT('',(-0.35,0.35,-4.28626379701573E-17));
#9676=CARTESIAN_POINT('Origin',(0.,0.35,0.));
#9677=CARTESIAN_POINT('',(-0.325,0.375,-3.9801020972289E-17));
#9678=CARTESIAN_POINT('Origin',(0.,0.19,0.));
#9679=CARTESIAN_POINT('',(-0.35,0.03,-4.28626379701574E-17));
#9680=CARTESIAN_POINT('Origin',(0.,0.03,0.));
#9681=CARTESIAN_POINT('',(-0.35,0.19,-4.28626379701574E-17));
#9682=CARTESIAN_POINT('Origin',(0.,0.0149999999999999,0.));
#9683=CARTESIAN_POINT('',(-0.32,-3.29597460435593E-17,-3.91886975727153E-17));
#9684=CARTESIAN_POINT('Origin',(0.,0.,0.));
#9685=CARTESIAN_POINT('',(-0.335,0.0149999999999999,-4.10256677714363E-17));
#9686=CARTESIAN_POINT('Origin',(0.22,0.,0.));
#9687=CARTESIAN_POINT('',(-0.22,-6.93889390390723E-18,-2.69422295812418E-17));
#9688=CARTESIAN_POINT('Origin',(0.,0.,0.));
#9689=CARTESIAN_POINT('Origin',(0.,-0.02,0.));
#9690=CARTESIAN_POINT('',(-0.1954,-0.0492,2.39295984553393E-17));
#9691=CARTESIAN_POINT('Origin',(0.,-0.0492,0.));
#9692=CARTESIAN_POINT('',(-0.21,-0.02,-2.57175827820944E-17));
#9693=CARTESIAN_POINT('Origin',(0.,-0.8,0.));
#9694=CARTESIAN_POINT('',(-0.1954,-0.8,-2.39295984553393E-17));
#9695=CARTESIAN_POINT('',(0.,0.,0.));
#9696=CARTESIAN_POINT('',(0.,0.,0.));
#9697=CARTESIAN_POINT('Origin',(0.,0.,0.));
#9698=CARTESIAN_POINT('',(-0.976185,-0.246528389340863,-1.19548183562566E-16));
#9699=CARTESIAN_POINT('',(-1.19548183562566E-16,-0.246528389340863,0.976185));
#9700=CARTESIAN_POINT('Origin',(0.,-0.246528389340863,0.));
#9701=CARTESIAN_POINT('Origin',(0.,-0.246528389340863,0.));
#9702=CARTESIAN_POINT('',(-1.19548183562566E-16,0.246528389340863,0.976185));
#9703=CARTESIAN_POINT('Origin',(-1.22464679914735E-16,0.,1.));
#9704=CARTESIAN_POINT('',(-0.976185,0.246528389340863,1.19548183562566E-16));
#9705=CARTESIAN_POINT('Origin',(0.,0.246528389340863,0.));
#9706=CARTESIAN_POINT('Origin',(0.,0.246528389340863,0.));
#9707=CARTESIAN_POINT('Origin',(0.,0.,0.));
#9708=CARTESIAN_POINT('',(-0.976185,0.45,-1.19548183562566E-16));
#9709=CARTESIAN_POINT('',(-0.976185,0.,-1.19548183562566E-16));
#9710=CARTESIAN_POINT('Origin',(0.,0.45,0.));
#9711=CARTESIAN_POINT('Origin',(0.,0.,0.));
#9712=CARTESIAN_POINT('',(-0.5,-0.39,-6.12323399573677E-17));
#9713=CARTESIAN_POINT('Origin',(0.,-0.39,0.));
#9714=CARTESIAN_POINT('',(-0.5,0.39,-6.12323399573677E-17));
#9715=CARTESIAN_POINT('',(-0.5,0.,-6.12323399573677E-17));
#9716=CARTESIAN_POINT('Origin',(0.,0.39,0.));
#9717=CARTESIAN_POINT('Origin',(0.,0.42,0.));
#9718=CARTESIAN_POINT('',(-0.56,0.45,-6.85802207522518E-17));
#9719=CARTESIAN_POINT('',(-0.53,0.42,-6.49062803548097E-17));
#9720=CARTESIAN_POINT('Origin',(0.,0.45,0.));
#9721=CARTESIAN_POINT('Origin',(0.976185,0.45,0.));
#9722=CARTESIAN_POINT('Origin',(0.,0.,0.));
#9723=CARTESIAN_POINT('',(-0.976185,-0.45,-1.19548183562566E-16));
#9724=CARTESIAN_POINT('Origin',(0.,-0.45,0.));
#9725=CARTESIAN_POINT('',(-0.976185,0.,-1.19548183562566E-16));
#9726=CARTESIAN_POINT('Origin',(0.56,-0.45,0.));
#9727=CARTESIAN_POINT('',(-0.56,-0.45,-6.85802207522518E-17));
#9728=CARTESIAN_POINT('Origin',(0.,-0.45,0.));
#9729=CARTESIAN_POINT('Origin',(0.,-0.42,0.));
#9730=CARTESIAN_POINT('',(-0.53,-0.42,-6.49062803548097E-17));
#9731=CARTESIAN_POINT('',(0.,0.,0.));
#9732=CARTESIAN_POINT('Origin',(0.,0.,0.));
#9733=CARTESIAN_POINT('',(-1.023815,0.246528389340863,-1.25381176266905E-16));
#9734=CARTESIAN_POINT('',(-1.25381176266905E-16,0.246528389340863,1.023815));
#9735=CARTESIAN_POINT('Origin',(0.,0.246528389340863,0.));
#9736=CARTESIAN_POINT('Origin',(0.,0.246528389340863,0.));
#9737=CARTESIAN_POINT('',(-1.25381176266905E-16,-0.246528389340863,1.023815));
#9738=CARTESIAN_POINT('Origin',(-1.22464679914735E-16,0.,1.));
#9739=CARTESIAN_POINT('',(-1.023815,-0.246528389340863,1.25381176266905E-16));
#9740=CARTESIAN_POINT('Origin',(0.,-0.246528389340863,0.));
#9741=CARTESIAN_POINT('Origin',(0.,-0.246528389340863,0.));
#9742=CARTESIAN_POINT('Origin',(0.,0.,0.));
#9743=CARTESIAN_POINT('',(-1.023815,-0.45,-1.25381176266905E-16));
#9744=CARTESIAN_POINT('Origin',(0.,-0.45,0.));
#9745=CARTESIAN_POINT('',(-1.023815,0.,-1.25381176266905E-16));
#9746=CARTESIAN_POINT('Origin',(1.44,0.45,0.));
#9747=CARTESIAN_POINT('',(-1.44,0.45,-1.76349139077219E-16));
#9748=CARTESIAN_POINT('Origin',(0.,0.45,0.));
#9749=CARTESIAN_POINT('',(-1.023815,0.45,-1.25381176266905E-16));
#9750=CARTESIAN_POINT('Origin',(0.,0.45,0.));
#9751=CARTESIAN_POINT('Origin',(0.,0.42,0.));
#9752=CARTESIAN_POINT('',(-1.5,0.39,-1.83697019872103E-16));
#9753=CARTESIAN_POINT('Origin',(0.,0.39,0.));
#9754=CARTESIAN_POINT('',(-1.47,0.42,-1.80023079474661E-16));
#9755=CARTESIAN_POINT('Origin',(0.,0.,0.));
#9756=CARTESIAN_POINT('',(-1.5,-0.39,-1.83697019872103E-16));
#9757=CARTESIAN_POINT('Origin',(0.,-0.39,0.));
#9758=CARTESIAN_POINT('',(-1.5,0.,-1.83697019872103E-16));
#9759=CARTESIAN_POINT('Origin',(0.,-0.42,0.));
#9760=CARTESIAN_POINT('',(-1.44,-0.45,-1.76349139077219E-16));
#9761=CARTESIAN_POINT('Origin',(0.,-0.45,0.));
#9762=CARTESIAN_POINT('',(-1.47,-0.42,-1.80023079474661E-16));
#9763=CARTESIAN_POINT('Origin',(1.023815,-0.45,0.));
#9764=CARTESIAN_POINT('Origin',(0.,0.,0.));
#9765=CARTESIAN_POINT('',(-1.023815,0.,-1.25381176266905E-16));
#9766=CARTESIAN_POINT('',(0.,0.,0.));
#9767=CARTESIAN_POINT('Origin',(1.,0.,0.));
#9768=CARTESIAN_POINT('',(1.,-1.78583896120461E-33,0.23815));
#9769=CARTESIAN_POINT('',(1.,-1.78583896120461E-33,-0.23815));
#9770=CARTESIAN_POINT('Origin',(1.,0.,0.));
#9771=CARTESIAN_POINT('Origin',(0.707106781186548,0.,-0.707106781186547));
#9772=CARTESIAN_POINT('',(0.875504261126124,-1.78583896120461E-33,-0.538709301246971));
#9773=CARTESIAN_POINT('',(0.538709301246971,-1.78583896120461E-33,-0.875504261126124));
#9774=CARTESIAN_POINT('Origin',(0.707106781186548,0.,-0.707106781186547));
#9775=CARTESIAN_POINT('Origin',(6.12323399573677E-17,0.,-1.));
#9776=CARTESIAN_POINT('',(0.23815,-1.78583896120461E-33,-1.));
#9777=CARTESIAN_POINT('',(-0.23815,-1.78583896120461E-33,-1.));
#9778=CARTESIAN_POINT('Origin',(6.12323399573677E-17,0.,-1.));
#9779=CARTESIAN_POINT('Origin',(-0.707106781186547,0.,-0.707106781186548));
#9780=CARTESIAN_POINT('',(-0.538709301246971,-1.78583896120461E-33,-0.875504261126124));
#9781=CARTESIAN_POINT('',(-0.875504261126124,-1.78583896120461E-33,-0.538709301246971));
#9782=CARTESIAN_POINT('Origin',(-0.707106781186547,0.,-0.707106781186548));
#9783=CARTESIAN_POINT('Origin',(-1.,0.,-1.22464679914735E-16));
#9784=CARTESIAN_POINT('',(-1.,-1.78583896120461E-33,-0.23815));
#9785=CARTESIAN_POINT('',(-1.,-1.78583896120461E-33,0.23815));
#9786=CARTESIAN_POINT('Origin',(-1.,0.,-1.22464679914735E-16));
#9787=CARTESIAN_POINT('Origin',(-0.707106781186548,0.,0.707106781186547));
#9788=CARTESIAN_POINT('',(-0.875504261126124,-7.94881478324376E-33,0.538709301246971));
#9789=CARTESIAN_POINT('',(-0.538709301246971,4.37713686083455E-33,0.875504261126124));
#9790=CARTESIAN_POINT('Origin',(-0.707106781186548,0.,0.707106781186547));
#9791=CARTESIAN_POINT('Origin',(-1.83697019872103E-16,0.,1.));
#9792=CARTESIAN_POINT('',(-0.23815,-1.78583896120461E-33,1.));
#9793=CARTESIAN_POINT('',(0.23815,-1.78583896120461E-33,1.));
#9794=CARTESIAN_POINT('Origin',(-1.83697019872103E-16,0.,1.));
#9795=CARTESIAN_POINT('Origin',(0.707106781186547,0.,0.707106781186548));
#9796=CARTESIAN_POINT('',(0.538709301246971,-4.86732687222419E-33,0.875504261126124));
#9797=CARTESIAN_POINT('',(0.875504261126124,1.29564894981497E-33,0.538709301246971));
#9798=CARTESIAN_POINT('Origin',(0.707106781186547,0.,0.707106781186548));
#9799=CARTESIAN_POINT('',(0.,0.,0.));
#9800=CARTESIAN_POINT('Origin',(0.707106781186547,0.,0.707106781186548));
#9801=CARTESIAN_POINT('',(0.504455939115715,-0.04763,0.841298510752802));
#9802=CARTESIAN_POINT('',(0.841298510752802,-0.04763,0.504455939115715));
#9803=CARTESIAN_POINT('Ctrl Pts',(0.504455939115715,-0.04763,0.841298510752802));
#9804=CARTESIAN_POINT('Ctrl Pts',(0.508899795931835,-0.0740444353928835,
0.838633903678357));
#9805=CARTESIAN_POINT('Ctrl Pts',(0.517157748491652,-0.0999305678883309,
0.833661031856294));
#9806=CARTESIAN_POINT('Ctrl Pts',(0.537715343527944,-0.142345102874864,
0.820511285096538));
#9807=CARTESIAN_POINT('Ctrl Pts',(0.548874290046456,-0.159766064500479,
0.813159949759));
#9808=CARTESIAN_POINT('Ctrl Pts',(0.573915184558107,-0.190326085855194,
0.795684265985089));
#9809=CARTESIAN_POINT('Ctrl Pts',(0.587792702767295,-0.203463743702801,
0.78555112003688));
#9810=CARTESIAN_POINT('Ctrl Pts',(0.615966552324775,-0.224161999508995,
0.763642258217233));
#9811=CARTESIAN_POINT('Ctrl Pts',(0.631684198665438,-0.232861760990032,
0.750785745543687));
#9812=CARTESIAN_POINT('Ctrl Pts',(0.663382628119203,-0.244251601209411,
0.722929908501543));
#9813=CARTESIAN_POINT('Ctrl Pts',(0.679352081686668,-0.246942143572133,
0.707917883896095));
#9814=CARTESIAN_POINT('Ctrl Pts',(0.707917883896095,-0.246942143572133,
0.679352081686668));
#9815=CARTESIAN_POINT('Ctrl Pts',(0.722929908501543,-0.244251601209411,
0.663382628119203));
#9816=CARTESIAN_POINT('Ctrl Pts',(0.750785745543687,-0.232861760990032,
0.631684198665439));
#9817=CARTESIAN_POINT('Ctrl Pts',(0.763642258217232,-0.224161999508995,
0.615966552324775));
#9818=CARTESIAN_POINT('Ctrl Pts',(0.78555112003688,-0.203463743702801,0.587792702767295));
#9819=CARTESIAN_POINT('Ctrl Pts',(0.795684265985088,-0.190326085855194,
0.573915184558108));
#9820=CARTESIAN_POINT('Ctrl Pts',(0.813159949759,-0.15976606450048,0.548874290046456));
#9821=CARTESIAN_POINT('Ctrl Pts',(0.820511285096538,-0.142345102874864,
0.537715343527944));
#9822=CARTESIAN_POINT('Ctrl Pts',(0.833661031856294,-0.099930567888331,
0.517157748491653));
#9823=CARTESIAN_POINT('Ctrl Pts',(0.838633903678357,-0.0740444353928835,
0.508899795931835));
#9824=CARTESIAN_POINT('Ctrl Pts',(0.841298510752801,-0.0476299999999999,
0.504455939115715));
#9825=CARTESIAN_POINT('',(0.528110872004958,-0.04763,0.871530771444223));
#9826=CARTESIAN_POINT('Origin',(0.707106781186547,-0.04763,0.707106781186548));
#9827=CARTESIAN_POINT('',(0.871530771444223,-0.04763,0.528110872004959));
#9828=CARTESIAN_POINT('Ctrl Pts',(0.871530771444223,-0.0476300000000001,
0.528110872004958));
#9829=CARTESIAN_POINT('Ctrl Pts',(0.87014664509073,-0.0609922781173483,
0.530395067942936));
#9830=CARTESIAN_POINT('Ctrl Pts',(0.868149331745851,-0.0742967091364493,
0.533674141594226));
#9831=CARTESIAN_POINT('Ctrl Pts',(0.85981294420286,-0.115492077056649,0.54708917182331));
#9832=CARTESIAN_POINT('Ctrl Pts',(0.850993704737257,-0.141695629206859,
0.560922177770136));
#9833=CARTESIAN_POINT('Ctrl Pts',(0.830754510485543,-0.181890537957859,
0.590422647829571));
#9834=CARTESIAN_POINT('Ctrl Pts',(0.816896541396381,-0.201072148666545,
0.609616703125488));
#9835=CARTESIAN_POINT('Ctrl Pts',(0.792310597819928,-0.223955109275652,
0.641117951819998));
#9836=CARTESIAN_POINT('Ctrl Pts',(0.779109323683612,-0.232742381310829,
0.657208095763053));
#9837=CARTESIAN_POINT('Ctrl Pts',(0.750552691816206,-0.244234834628584,
0.68964083160521));
#9838=CARTESIAN_POINT('Ctrl Pts',(0.735185187071673,-0.246942143572133,
0.705971972091755));
#9839=CARTESIAN_POINT('Ctrl Pts',(0.705971972091754,-0.246942143572133,
0.735185187071673));
#9840=CARTESIAN_POINT('Ctrl Pts',(0.689640831605209,-0.244234834628584,
0.750552691816206));
#9841=CARTESIAN_POINT('Ctrl Pts',(0.657208095763052,-0.232742381310829,
0.779109323683612));
#9842=CARTESIAN_POINT('Ctrl Pts',(0.641117951819998,-0.223955109275652,
0.792310597819928));
#9843=CARTESIAN_POINT('Ctrl Pts',(0.609616703125487,-0.201072148666545,
0.816896541396382));
#9844=CARTESIAN_POINT('Ctrl Pts',(0.590422647829571,-0.181890537957858,
0.830754510485544));
#9845=CARTESIAN_POINT('Ctrl Pts',(0.560922177770135,-0.141695629206858,
0.850993704737257));
#9846=CARTESIAN_POINT('Ctrl Pts',(0.547089171823309,-0.115492077056649,
0.859812944202861));
#9847=CARTESIAN_POINT('Ctrl Pts',(0.533674141594226,-0.0742967091364491,
0.868149331745852));
#9848=CARTESIAN_POINT('Ctrl Pts',(0.530395067942936,-0.0609922781173483,
0.870146645090731));
#9849=CARTESIAN_POINT('Ctrl Pts',(0.528110872004958,-0.0476300000000001,
0.871530771444223));
#9850=CARTESIAN_POINT('Origin',(0.707106781186547,-0.04763,0.707106781186548));
#9851=CARTESIAN_POINT('Origin',(0.,-0.166705,0.));
#9852=CARTESIAN_POINT('',(0.242834539687906,-0.04763,0.989696097314));
#9853=CARTESIAN_POINT('Origin',(0.,-0.04763,0.));
#9854=CARTESIAN_POINT('',(-0.242834539687907,-0.04763,0.989696097314));
#9855=CARTESIAN_POINT('Ctrl Pts',(0.242834539687906,-0.04763,0.989696097314));
#9856=CARTESIAN_POINT('Ctrl Pts',(0.24024064412003,-0.0609922781173483,
0.990332542620729));
#9857=CARTESIAN_POINT('Ctrl Pts',(0.236509675094874,-0.0742967091364492,
0.991238884025248));
#9858=CARTESIAN_POINT('Ctrl Pts',(0.221129100087819,-0.115492077056649,
0.994830026707808));
#9859=CARTESIAN_POINT('Ctrl Pts',(0.205111543747588,-0.141695629206859,
0.998375294985966));
#9860=CARTESIAN_POINT('Ctrl Pts',(0.169940289819232,-0.181890537957859,
1.00492400591205));
#9861=CARTESIAN_POINT('Ctrl Pts',(0.1465689792446,-0.201072148666545,1.00869718865384));
#9862=CARTESIAN_POINT('Ctrl Pts',(0.106909345252087,-0.223955109275652,
1.01358704779679));
#9863=CARTESIAN_POINT('Ctrl Pts',(0.0861971848975941,-0.232742381310829,
1.0156297872271));
#9864=CARTESIAN_POINT('Ctrl Pts',(0.0430711894098822,-0.244234834628584,
1.01837060663223));
#9865=CARTESIAN_POINT('Ctrl Pts',(0.0206568624125605,-0.246942143572133,
1.019052));
#9866=CARTESIAN_POINT('Ctrl Pts',(-0.0206568624125608,-0.246942143572133,
1.019052));
#9867=CARTESIAN_POINT('Ctrl Pts',(-0.0430711894098825,-0.244234834628584,
1.01837060663223));
#9868=CARTESIAN_POINT('Ctrl Pts',(-0.0861971848975943,-0.232742381310829,
1.0156297872271));
#9869=CARTESIAN_POINT('Ctrl Pts',(-0.106909345252088,-0.223955109275652,
1.01358704779679));
#9870=CARTESIAN_POINT('Ctrl Pts',(-0.1465689792446,-0.201072148666545,1.00869718865384));
#9871=CARTESIAN_POINT('Ctrl Pts',(-0.169940289819232,-0.181890537957859,
1.00492400591205));
#9872=CARTESIAN_POINT('Ctrl Pts',(-0.205111543747588,-0.141695629206859,
0.998375294985966));
#9873=CARTESIAN_POINT('Ctrl Pts',(-0.221129100087819,-0.115492077056649,
0.994830026707808));
#9874=CARTESIAN_POINT('Ctrl Pts',(-0.236509675094875,-0.0742967091364493,
0.991238884025248));
#9875=CARTESIAN_POINT('Ctrl Pts',(-0.24024064412003,-0.0609922781173483,
0.990332542620729));
#9876=CARTESIAN_POINT('Ctrl Pts',(-0.242834539687907,-0.04763,0.989696097314));
#9877=CARTESIAN_POINT('',(-0.528110872004959,-0.04763,0.871530771444223));
#9878=CARTESIAN_POINT('Origin',(0.,-0.04763,0.));
#9879=CARTESIAN_POINT('',(-0.871530771444223,-0.04763,0.528110872004958));
#9880=CARTESIAN_POINT('Ctrl Pts',(-0.528110872004958,-0.0476300000000001,
0.871530771444223));
#9881=CARTESIAN_POINT('Ctrl Pts',(-0.530395067942936,-0.0609922781173484,
0.87014664509073));
#9882=CARTESIAN_POINT('Ctrl Pts',(-0.533674141594226,-0.0742967091364493,
0.868149331745851));
#9883=CARTESIAN_POINT('Ctrl Pts',(-0.54708917182331,-0.115492077056649,
0.85981294420286));
#9884=CARTESIAN_POINT('Ctrl Pts',(-0.560922177770136,-0.141695629206859,
0.850993704737257));
#9885=CARTESIAN_POINT('Ctrl Pts',(-0.590422647829571,-0.181890537957859,
0.830754510485543));
#9886=CARTESIAN_POINT('Ctrl Pts',(-0.609616703125488,-0.201072148666545,
0.816896541396381));
#9887=CARTESIAN_POINT('Ctrl Pts',(-0.641117951819998,-0.223955109275652,
0.792310597819928));
#9888=CARTESIAN_POINT('Ctrl Pts',(-0.657208095763053,-0.232742381310829,
0.779109323683611));
#9889=CARTESIAN_POINT('Ctrl Pts',(-0.68964083160521,-0.244234834628584,
0.750552691816205));
#9890=CARTESIAN_POINT('Ctrl Pts',(-0.705971972091755,-0.246942143572133,
0.735185187071673));
#9891=CARTESIAN_POINT('Ctrl Pts',(-0.735185187071673,-0.246942143572133,
0.705971972091754));
#9892=CARTESIAN_POINT('Ctrl Pts',(-0.750552691816206,-0.244234834628584,
0.689640831605209));
#9893=CARTESIAN_POINT('Ctrl Pts',(-0.779109323683612,-0.232742381310829,
0.657208095763052));
#9894=CARTESIAN_POINT('Ctrl Pts',(-0.792310597819928,-0.223955109275652,
0.641117951819998));
#9895=CARTESIAN_POINT('Ctrl Pts',(-0.816896541396382,-0.201072148666545,
0.609616703125487));
#9896=CARTESIAN_POINT('Ctrl Pts',(-0.830754510485544,-0.181890537957858,
0.590422647829571));
#9897=CARTESIAN_POINT('Ctrl Pts',(-0.850993704737257,-0.141695629206858,
0.560922177770135));
#9898=CARTESIAN_POINT('Ctrl Pts',(-0.859812944202861,-0.115492077056649,
0.547089171823309));
#9899=CARTESIAN_POINT('Ctrl Pts',(-0.868149331745852,-0.0742967091364491,
0.533674141594226));
#9900=CARTESIAN_POINT('Ctrl Pts',(-0.870146645090731,-0.0609922781173483,
0.530395067942936));
#9901=CARTESIAN_POINT('Ctrl Pts',(-0.871530771444223,-0.04763,0.528110872004958));
#9902=CARTESIAN_POINT('',(-0.989696097314,-0.04763,0.242834539687906));
#9903=CARTESIAN_POINT('Origin',(0.,-0.04763,0.));
#9904=CARTESIAN_POINT('',(-1.019052,-0.246942143572133,1.248489836334E-16));
#9905=CARTESIAN_POINT('Ctrl Pts',(-0.989696097314,-0.04763,0.242834539687906));
#9906=CARTESIAN_POINT('Ctrl Pts',(-0.990332542620729,-0.0609922781173483,
0.24024064412003));
#9907=CARTESIAN_POINT('Ctrl Pts',(-0.991238884025248,-0.0742967091364492,
0.236509675094874));
#9908=CARTESIAN_POINT('Ctrl Pts',(-0.994830026707808,-0.115492077056649,
0.221129100087819));
#9909=CARTESIAN_POINT('Ctrl Pts',(-0.998375294985966,-0.141695629206859,
0.205111543747588));
#9910=CARTESIAN_POINT('Ctrl Pts',(-1.00492400591205,-0.181890537957859,
0.169940289819232));
#9911=CARTESIAN_POINT('Ctrl Pts',(-1.00869718865384,-0.201072148666545,
0.1465689792446));
#9912=CARTESIAN_POINT('Ctrl Pts',(-1.01358704779679,-0.223955109275652,
0.106909345252088));
#9913=CARTESIAN_POINT('Ctrl Pts',(-1.0156297872271,-0.232742381310829,0.0861971848975944));
#9914=CARTESIAN_POINT('Ctrl Pts',(-1.01837060663223,-0.244234834628584,
0.0430711894098825));
#9915=CARTESIAN_POINT('Ctrl Pts',(-1.019052,-0.246942143572133,0.0206568624125608));
#9916=CARTESIAN_POINT('Ctrl Pts',(-1.019052,-0.246942143572133,1.2490009027033E-16));
#9917=CARTESIAN_POINT('',(-1.019052,-0.28578,1.24797876996471E-16));
#9918=CARTESIAN_POINT('',(-1.019052,-0.166705,1.24797876996471E-16));
#9919=CARTESIAN_POINT('Origin',(0.,-0.28578,0.));
#9920=CARTESIAN_POINT('',(-0.989696097314,-0.04763,-0.242834539687906));
#9921=CARTESIAN_POINT('Ctrl Pts',(-1.019052,-0.246942143572133,1.2490009027033E-16));
#9922=CARTESIAN_POINT('Ctrl Pts',(-1.019052,-0.246942143572133,-0.0206568624125605));
#9923=CARTESIAN_POINT('Ctrl Pts',(-1.01837060663223,-0.244234834628584,
-0.0430711894098822));
#9924=CARTESIAN_POINT('Ctrl Pts',(-1.0156297872271,-0.232742381310829,-0.0861971848975941));
#9925=CARTESIAN_POINT('Ctrl Pts',(-1.01358704779679,-0.223955109275652,
-0.106909345252087));
#9926=CARTESIAN_POINT('Ctrl Pts',(-1.00869718865384,-0.201072148666546,
-0.1465689792446));
#9927=CARTESIAN_POINT('Ctrl Pts',(-1.00492400591205,-0.181890537957859,
-0.169940289819232));
#9928=CARTESIAN_POINT('Ctrl Pts',(-0.998375294985966,-0.141695629206859,
-0.205111543747588));
#9929=CARTESIAN_POINT('Ctrl Pts',(-0.994830026707808,-0.11549207705665,
-0.221129100087819));
#9930=CARTESIAN_POINT('Ctrl Pts',(-0.991238884025248,-0.0742967091364495,
-0.236509675094874));
#9931=CARTESIAN_POINT('Ctrl Pts',(-0.990332542620729,-0.0609922781173484,
-0.24024064412003));
#9932=CARTESIAN_POINT('Ctrl Pts',(-0.989696097314,-0.0476300000000001,-0.242834539687907));
#9933=CARTESIAN_POINT('',(-0.871530771444223,-0.04763,-0.528110872004958));
#9934=CARTESIAN_POINT('Origin',(0.,-0.04763,0.));
#9935=CARTESIAN_POINT('',(-0.528110872004958,-0.04763,-0.871530771444223));
#9936=CARTESIAN_POINT('Ctrl Pts',(-0.871530771444223,-0.0476300000000001,
-0.528110872004958));
#9937=CARTESIAN_POINT('Ctrl Pts',(-0.87014664509073,-0.0609922781173484,
-0.530395067942936));
#9938=CARTESIAN_POINT('Ctrl Pts',(-0.868149331745851,-0.0742967091364494,
-0.533674141594226));
#9939=CARTESIAN_POINT('Ctrl Pts',(-0.85981294420286,-0.115492077056649,
-0.54708917182331));
#9940=CARTESIAN_POINT('Ctrl Pts',(-0.850993704737257,-0.141695629206859,
-0.560922177770136));
#9941=CARTESIAN_POINT('Ctrl Pts',(-0.830754510485543,-0.181890537957859,
-0.590422647829571));
#9942=CARTESIAN_POINT('Ctrl Pts',(-0.816896541396381,-0.201072148666546,
-0.609616703125488));
#9943=CARTESIAN_POINT('Ctrl Pts',(-0.792310597819928,-0.223955109275652,
-0.641117951819999));
#9944=CARTESIAN_POINT('Ctrl Pts',(-0.779109323683611,-0.232742381310829,
-0.657208095763053));
#9945=CARTESIAN_POINT('Ctrl Pts',(-0.750552691816205,-0.244234834628584,
-0.68964083160521));
#9946=CARTESIAN_POINT('Ctrl Pts',(-0.735185187071673,-0.246942143572133,
-0.705971972091755));
#9947=CARTESIAN_POINT('Ctrl Pts',(-0.705971972091754,-0.246942143572133,
-0.735185187071673));
#9948=CARTESIAN_POINT('Ctrl Pts',(-0.68964083160521,-0.244234834628584,
-0.750552691816206));
#9949=CARTESIAN_POINT('Ctrl Pts',(-0.657208095763052,-0.232742381310829,
-0.779109323683612));
#9950=CARTESIAN_POINT('Ctrl Pts',(-0.641117951819998,-0.223955109275652,
-0.792310597819928));
#9951=CARTESIAN_POINT('Ctrl Pts',(-0.609616703125488,-0.201072148666545,
-0.816896541396381));
#9952=CARTESIAN_POINT('Ctrl Pts',(-0.590422647829571,-0.181890537957859,
-0.830754510485543));
#9953=CARTESIAN_POINT('Ctrl Pts',(-0.560922177770136,-0.141695629206859,
-0.850993704737257));
#9954=CARTESIAN_POINT('Ctrl Pts',(-0.54708917182331,-0.115492077056649,
-0.85981294420286));
#9955=CARTESIAN_POINT('Ctrl Pts',(-0.533674141594226,-0.0742967091364494,
-0.868149331745852));
#9956=CARTESIAN_POINT('Ctrl Pts',(-0.530395067942936,-0.0609922781173484,
-0.870146645090731));
#9957=CARTESIAN_POINT('Ctrl Pts',(-0.528110872004958,-0.0476300000000001,
-0.871530771444223));
#9958=CARTESIAN_POINT('',(-0.242834539687906,-0.04763,-0.989696097314));
#9959=CARTESIAN_POINT('Origin',(0.,-0.04763,0.));
#9960=CARTESIAN_POINT('',(0.242834539687906,-0.04763,-0.989696097314));
#9961=CARTESIAN_POINT('Ctrl Pts',(-0.242834539687907,-0.04763,-0.989696097314));
#9962=CARTESIAN_POINT('Ctrl Pts',(-0.24024064412003,-0.0609922781173483,
-0.990332542620729));
#9963=CARTESIAN_POINT('Ctrl Pts',(-0.236509675094874,-0.0742967091364493,
-0.991238884025248));
#9964=CARTESIAN_POINT('Ctrl Pts',(-0.221129100087819,-0.115492077056649,
-0.994830026707808));
#9965=CARTESIAN_POINT('Ctrl Pts',(-0.205111543747588,-0.141695629206859,
-0.998375294985966));
#9966=CARTESIAN_POINT('Ctrl Pts',(-0.169940289819232,-0.181890537957859,
-1.00492400591205));
#9967=CARTESIAN_POINT('Ctrl Pts',(-0.1465689792446,-0.201072148666545,-1.00869718865384));
#9968=CARTESIAN_POINT('Ctrl Pts',(-0.106909345252087,-0.223955109275652,
-1.01358704779679));
#9969=CARTESIAN_POINT('Ctrl Pts',(-0.0861971848975942,-0.232742381310829,
-1.0156297872271));
#9970=CARTESIAN_POINT('Ctrl Pts',(-0.0430711894098823,-0.244234834628584,
-1.01837060663223));
#9971=CARTESIAN_POINT('Ctrl Pts',(-0.0206568624125606,-0.246942143572133,
-1.019052));
#9972=CARTESIAN_POINT('Ctrl Pts',(0.0206568624125607,-0.246942143572133,
-1.019052));
#9973=CARTESIAN_POINT('Ctrl Pts',(0.0430711894098824,-0.244234834628584,
-1.01837060663223));
#9974=CARTESIAN_POINT('Ctrl Pts',(0.0861971848975943,-0.232742381310829,
-1.0156297872271));
#9975=CARTESIAN_POINT('Ctrl Pts',(0.106909345252088,-0.223955109275652,
-1.01358704779679));
#9976=CARTESIAN_POINT('Ctrl Pts',(0.1465689792446,-0.201072148666545,-1.00869718865384));
#9977=CARTESIAN_POINT('Ctrl Pts',(0.169940289819232,-0.181890537957859,
-1.00492400591205));
#9978=CARTESIAN_POINT('Ctrl Pts',(0.205111543747588,-0.141695629206859,
-0.998375294985966));
#9979=CARTESIAN_POINT('Ctrl Pts',(0.221129100087819,-0.115492077056649,
-0.994830026707808));
#9980=CARTESIAN_POINT('Ctrl Pts',(0.236509675094874,-0.0742967091364493,
-0.991238884025248));
#9981=CARTESIAN_POINT('Ctrl Pts',(0.24024064412003,-0.0609922781173484,
-0.990332542620729));
#9982=CARTESIAN_POINT('Ctrl Pts',(0.242834539687907,-0.04763,-0.989696097314));
#9983=CARTESIAN_POINT('',(0.528110872004958,-0.04763,-0.871530771444223));
#9984=CARTESIAN_POINT('Origin',(0.,-0.04763,0.));
#9985=CARTESIAN_POINT('',(0.871530771444223,-0.04763,-0.528110872004958));
#9986=CARTESIAN_POINT('Ctrl Pts',(0.528110872004958,-0.0476300000000001,
-0.871530771444223));
#9987=CARTESIAN_POINT('Ctrl Pts',(0.530395067942936,-0.0609922781173484,
-0.870146645090731));
#9988=CARTESIAN_POINT('Ctrl Pts',(0.533674141594226,-0.0742967091364493,
-0.868149331745851));
#9989=CARTESIAN_POINT('Ctrl Pts',(0.54708917182331,-0.115492077056649,-0.85981294420286));
#9990=CARTESIAN_POINT('Ctrl Pts',(0.560922177770136,-0.141695629206859,
-0.850993704737257));
#9991=CARTESIAN_POINT('Ctrl Pts',(0.590422647829571,-0.181890537957859,
-0.830754510485543));
#9992=CARTESIAN_POINT('Ctrl Pts',(0.609616703125488,-0.201072148666545,
-0.816896541396381));
#9993=CARTESIAN_POINT('Ctrl Pts',(0.641117951819998,-0.223955109275652,
-0.792310597819928));
#9994=CARTESIAN_POINT('Ctrl Pts',(0.657208095763053,-0.232742381310829,
-0.779109323683612));
#9995=CARTESIAN_POINT('Ctrl Pts',(0.68964083160521,-0.244234834628584,-0.750552691816206));
#9996=CARTESIAN_POINT('Ctrl Pts',(0.705971972091755,-0.246942143572133,
-0.735185187071673));
#9997=CARTESIAN_POINT('Ctrl Pts',(0.735185187071673,-0.246942143572133,
-0.705971972091754));
#9998=CARTESIAN_POINT('Ctrl Pts',(0.750552691816206,-0.244234834628584,
-0.68964083160521));
#9999=CARTESIAN_POINT('Ctrl Pts',(0.779109323683612,-0.232742381310829,
-0.657208095763053));
#10000=CARTESIAN_POINT('Ctrl Pts',(0.792310597819928,-0.223955109275652,
-0.641117951819998));
#10001=CARTESIAN_POINT('Ctrl Pts',(0.816896541396381,-0.201072148666545,
-0.609616703125488));
#10002=CARTESIAN_POINT('Ctrl Pts',(0.830754510485543,-0.181890537957859,
-0.590422647829571));
#10003=CARTESIAN_POINT('Ctrl Pts',(0.850993704737257,-0.141695629206859,
-0.560922177770136));
#10004=CARTESIAN_POINT('Ctrl Pts',(0.85981294420286,-0.115492077056649,
-0.54708917182331));
#10005=CARTESIAN_POINT('Ctrl Pts',(0.868149331745851,-0.0742967091364493,
-0.533674141594226));
#10006=CARTESIAN_POINT('Ctrl Pts',(0.870146645090731,-0.0609922781173484,
-0.530395067942936));
#10007=CARTESIAN_POINT('Ctrl Pts',(0.871530771444223,-0.0476300000000001,
-0.528110872004958));
#10008=CARTESIAN_POINT('',(0.989696097314,-0.04763,-0.242834539687906));
#10009=CARTESIAN_POINT('Origin',(0.,-0.04763,0.));
#10010=CARTESIAN_POINT('',(0.989696097314,-0.04763,0.242834539687906));
#10011=CARTESIAN_POINT('Ctrl Pts',(0.989696097314,-0.04763,-0.242834539687907));
#10012=CARTESIAN_POINT('Ctrl Pts',(0.990332542620729,-0.0609922781173483,
-0.24024064412003));
#10013=CARTESIAN_POINT('Ctrl Pts',(0.991238884025248,-0.0742967091364493,
-0.236509675094874));
#10014=CARTESIAN_POINT('Ctrl Pts',(0.994830026707808,-0.115492077056649,
-0.221129100087819));
#10015=CARTESIAN_POINT('Ctrl Pts',(0.998375294985966,-0.141695629206859,
-0.205111543747588));
#10016=CARTESIAN_POINT('Ctrl Pts',(1.00492400591205,-0.181890537957859,
-0.169940289819232));
#10017=CARTESIAN_POINT('Ctrl Pts',(1.00869718865384,-0.201072148666545,
-0.1465689792446));
#10018=CARTESIAN_POINT('Ctrl Pts',(1.01358704779679,-0.223955109275652,
-0.106909345252087));
#10019=CARTESIAN_POINT('Ctrl Pts',(1.0156297872271,-0.232742381310829,-0.0861971848975942));
#10020=CARTESIAN_POINT('Ctrl Pts',(1.01837060663223,-0.244234834628584,
-0.0430711894098823));
#10021=CARTESIAN_POINT('Ctrl Pts',(1.019052,-0.246942143572133,-0.0206568624125607));
#10022=CARTESIAN_POINT('Ctrl Pts',(1.019052,-0.246942143572133,0.0206568624125607));
#10023=CARTESIAN_POINT('Ctrl Pts',(1.01837060663223,-0.244234834628584,
0.0430711894098823));
#10024=CARTESIAN_POINT('Ctrl Pts',(1.0156297872271,-0.232742381310829,0.0861971848975942));
#10025=CARTESIAN_POINT('Ctrl Pts',(1.01358704779679,-0.223955109275652,
0.106909345252087));
#10026=CARTESIAN_POINT('Ctrl Pts',(1.00869718865384,-0.201072148666545,
0.1465689792446));
#10027=CARTESIAN_POINT('Ctrl Pts',(1.00492400591205,-0.181890537957859,
0.169940289819232));
#10028=CARTESIAN_POINT('Ctrl Pts',(0.998375294985966,-0.141695629206859,
0.205111543747588));
#10029=CARTESIAN_POINT('Ctrl Pts',(0.994830026707808,-0.115492077056649,
0.221129100087819));
#10030=CARTESIAN_POINT('Ctrl Pts',(0.991238884025248,-0.0742967091364492,
0.236509675094874));
#10031=CARTESIAN_POINT('Ctrl Pts',(0.990332542620729,-0.0609922781173483,
0.24024064412003));
#10032=CARTESIAN_POINT('Ctrl Pts',(0.989696097314,-0.04763,0.242834539687907));
#10033=CARTESIAN_POINT('Origin',(0.,-0.04763,0.));
#10034=CARTESIAN_POINT('Origin',(0.,-0.04763,0.));
#10035=CARTESIAN_POINT('',(0.238183666596899,-0.04763,0.951592097314));
#10036=CARTESIAN_POINT('Origin',(0.,-0.04763,0.));
#10037=CARTESIAN_POINT('Origin',(-1.94289029309402E-16,-0.04763,1.));
#10038=CARTESIAN_POINT('Origin',(-1.94289029309402E-16,0.,1.));
#10039=CARTESIAN_POINT('',(-0.2381836665969,-0.04763,0.951592097314));
#10040=CARTESIAN_POINT('Ctrl Pts',(-0.238183666596899,-0.0476299999999999,
0.951592097314));
#10041=CARTESIAN_POINT('Ctrl Pts',(-0.233157223576062,-0.0740444353928835,
0.952850216871763));
#10042=CARTESIAN_POINT('Ctrl Pts',(-0.223801617934946,-0.0999305678883309,
0.955173119738174));
#10043=CARTESIAN_POINT('Ctrl Pts',(-0.199966927975188,-0.142345102874864,
0.960411259488514));
#10044=CARTESIAN_POINT('Ctrl Pts',(-0.1868781821531,-0.159766064500479,
0.963103647174702));
#10045=CARTESIAN_POINT('Ctrl Pts',(-0.15681442133453,-0.190326085855194,
0.968453058988463));
#10046=CARTESIAN_POINT('Ctrl Pts',(-0.139836317888043,-0.203463743702801,
0.971100730005489));
#10047=CARTESIAN_POINT('Ctrl Pts',(-0.104422493053067,-0.224161999508995,
0.975530745318961));
#10048=CARTESIAN_POINT('Ctrl Pts',(-0.0842175114474176,-0.232861760990032,
0.977553872336861));
#10049=CARTESIAN_POINT('Ctrl Pts',(-0.0421062857595701,-0.244251601209411,
0.980270995488453));
#10050=CARTESIAN_POINT('Ctrl Pts',(-0.0201990724523197,-0.246942143572133,
0.980948));
#10051=CARTESIAN_POINT('Ctrl Pts',(0.020199072452319,-0.246942143572133,
0.980948));
#10052=CARTESIAN_POINT('Ctrl Pts',(0.0421062857595694,-0.244251601209411,
0.980270995488454));
#10053=CARTESIAN_POINT('Ctrl Pts',(0.0842175114474169,-0.232861760990032,
0.977553872336861));
#10054=CARTESIAN_POINT('Ctrl Pts',(0.104422493053067,-0.224161999508995,
0.975530745318961));
#10055=CARTESIAN_POINT('Ctrl Pts',(0.139836317888042,-0.203463743702801,
0.971100730005489));
#10056=CARTESIAN_POINT('Ctrl Pts',(0.15681442133453,-0.190326085855194,
0.968453058988463));
#10057=CARTESIAN_POINT('Ctrl Pts',(0.1868781821531,-0.15976606450048,0.963103647174702));
#10058=CARTESIAN_POINT('Ctrl Pts',(0.199966927975188,-0.142345102874864,
0.960411259488514));
#10059=CARTESIAN_POINT('Ctrl Pts',(0.223801617934945,-0.0999305678883309,
0.955173119738174));
#10060=CARTESIAN_POINT('Ctrl Pts',(0.233157223576061,-0.0740444353928835,
0.952850216871763));
#10061=CARTESIAN_POINT('Ctrl Pts',(0.238183666596899,-0.0476299999999999,
0.951592097314));
#10062=CARTESIAN_POINT('Origin',(-1.94289029309402E-16,-0.04763,1.));
#10063=CARTESIAN_POINT('Origin',(0.,-0.04763,0.));
#10064=CARTESIAN_POINT('',(-0.504455939115715,-0.04763,0.841298510752802));
#10065=CARTESIAN_POINT('Origin',(0.,-0.04763,0.));
#10066=CARTESIAN_POINT('Origin',(-0.707106781186548,-0.04763,0.707106781186547));
#10067=CARTESIAN_POINT('Origin',(-0.707106781186548,0.,0.707106781186547));
#10068=CARTESIAN_POINT('',(-0.841298510752802,-0.04763,0.504455939115715));
#10069=CARTESIAN_POINT('Ctrl Pts',(-0.841298510752802,-0.04763,0.504455939115715));
#10070=CARTESIAN_POINT('Ctrl Pts',(-0.838633903678357,-0.0740444353928835,
0.508899795931835));
#10071=CARTESIAN_POINT('Ctrl Pts',(-0.833661031856294,-0.0999305678883309,
0.517157748491652));
#10072=CARTESIAN_POINT('Ctrl Pts',(-0.820511285096538,-0.142345102874864,
0.537715343527944));
#10073=CARTESIAN_POINT('Ctrl Pts',(-0.813159949759,-0.159766064500479,0.548874290046456));
#10074=CARTESIAN_POINT('Ctrl Pts',(-0.795684265985089,-0.190326085855194,
0.573915184558107));
#10075=CARTESIAN_POINT('Ctrl Pts',(-0.78555112003688,-0.203463743702801,
0.587792702767295));
#10076=CARTESIAN_POINT('Ctrl Pts',(-0.763642258217233,-0.224161999508995,
0.615966552324775));
#10077=CARTESIAN_POINT('Ctrl Pts',(-0.750785745543687,-0.232861760990032,
0.631684198665438));
#10078=CARTESIAN_POINT('Ctrl Pts',(-0.722929908501543,-0.244251601209411,
0.663382628119203));
#10079=CARTESIAN_POINT('Ctrl Pts',(-0.707917883896095,-0.246942143572133,
0.679352081686668));
#10080=CARTESIAN_POINT('Ctrl Pts',(-0.679352081686668,-0.246942143572133,
0.707917883896095));
#10081=CARTESIAN_POINT('Ctrl Pts',(-0.663382628119203,-0.244251601209411,
0.722929908501544));
#10082=CARTESIAN_POINT('Ctrl Pts',(-0.631684198665438,-0.232861760990031,
0.750785745543687));
#10083=CARTESIAN_POINT('Ctrl Pts',(-0.615966552324775,-0.224161999508995,
0.763642258217233));
#10084=CARTESIAN_POINT('Ctrl Pts',(-0.587792702767295,-0.203463743702801,
0.78555112003688));
#10085=CARTESIAN_POINT('Ctrl Pts',(-0.573915184558107,-0.190326085855194,
0.795684265985088));
#10086=CARTESIAN_POINT('Ctrl Pts',(-0.548874290046456,-0.159766064500479,
0.813159949759));
#10087=CARTESIAN_POINT('Ctrl Pts',(-0.537715343527944,-0.142345102874864,
0.820511285096538));
#10088=CARTESIAN_POINT('Ctrl Pts',(-0.517157748491652,-0.0999305678883309,
0.833661031856294));
#10089=CARTESIAN_POINT('Ctrl Pts',(-0.508899795931835,-0.0740444353928835,
0.838633903678357));
#10090=CARTESIAN_POINT('Ctrl Pts',(-0.504455939115716,-0.04763,0.841298510752801));
#10091=CARTESIAN_POINT('Origin',(-0.707106781186548,-0.04763,0.707106781186547));
#10092=CARTESIAN_POINT('Origin',(0.,-0.04763,0.));
#10093=CARTESIAN_POINT('',(-0.951592097314,-0.04763,0.238183666596899));
#10094=CARTESIAN_POINT('Origin',(0.,-0.04763,0.));
#10095=CARTESIAN_POINT('Origin',(-1.,-0.04763,-1.11022302462516E-16));
#10096=CARTESIAN_POINT('Origin',(-1.,0.,-1.11022302462516E-16));
#10097=CARTESIAN_POINT('',(-0.951592097314,-0.04763,-0.2381836665969));
#10098=CARTESIAN_POINT('',(-0.980948,-0.246942143572133,1.08514323328844E-18));
#10099=CARTESIAN_POINT('Ctrl Pts',(-0.951592097314,-0.04763,-0.238183666596899));
#10100=CARTESIAN_POINT('Ctrl Pts',(-0.952850216871763,-0.0740444353928835,
-0.233157223576062));
#10101=CARTESIAN_POINT('Ctrl Pts',(-0.955173119738174,-0.0999305678883309,
-0.223801617934946));
#10102=CARTESIAN_POINT('Ctrl Pts',(-0.960411259488514,-0.142345102874864,
-0.199966927975188));
#10103=CARTESIAN_POINT('Ctrl Pts',(-0.963103647174702,-0.159766064500479,
-0.1868781821531));
#10104=CARTESIAN_POINT('Ctrl Pts',(-0.968453058988463,-0.190326085855194,
-0.15681442133453));
#10105=CARTESIAN_POINT('Ctrl Pts',(-0.971100730005489,-0.203463743702801,
-0.139836317888043));
#10106=CARTESIAN_POINT('Ctrl Pts',(-0.975530745318961,-0.224161999508995,
-0.104422493053067));
#10107=CARTESIAN_POINT('Ctrl Pts',(-0.977553872336861,-0.232861760990032,
-0.0842175114474175));
#10108=CARTESIAN_POINT('Ctrl Pts',(-0.980270995488453,-0.244251601209411,
-0.0421062857595699));
#10109=CARTESIAN_POINT('Ctrl Pts',(-0.980948,-0.246942143572133,-0.0201990724523195));
#10110=CARTESIAN_POINT('Ctrl Pts',(-0.980948,-0.246942143572133,-1.17961196366423E-16));
#10111=CARTESIAN_POINT('Origin',(-1.,-0.04763,-1.11022302462516E-16));
#10112=CARTESIAN_POINT('Ctrl Pts',(-0.980948,-0.246942143572133,-1.17961196366423E-16));
#10113=CARTESIAN_POINT('Ctrl Pts',(-0.980948,-0.246942143572133,0.0201990724523192));
#10114=CARTESIAN_POINT('Ctrl Pts',(-0.980270995488453,-0.244251601209411,
0.0421062857595695));
#10115=CARTESIAN_POINT('Ctrl Pts',(-0.977553872336861,-0.232861760990032,
0.0842175114474169));
#10116=CARTESIAN_POINT('Ctrl Pts',(-0.975530745318961,-0.224161999508995,
0.104422493053066));
#10117=CARTESIAN_POINT('Ctrl Pts',(-0.971100730005489,-0.203463743702801,
0.139836317888042));
#10118=CARTESIAN_POINT('Ctrl Pts',(-0.968453058988463,-0.190326085855194,
0.15681442133453));
#10119=CARTESIAN_POINT('Ctrl Pts',(-0.963103647174702,-0.15976606450048,
0.1868781821531));
#10120=CARTESIAN_POINT('Ctrl Pts',(-0.960411259488514,-0.142345102874864,
0.199966927975188));
#10121=CARTESIAN_POINT('Ctrl Pts',(-0.955173119738174,-0.099930567888331,
0.223801617934945));
#10122=CARTESIAN_POINT('Ctrl Pts',(-0.952850216871763,-0.0740444353928835,
0.233157223576061));
#10123=CARTESIAN_POINT('Ctrl Pts',(-0.951592097314,-0.04763,0.238183666596899));
#10124=CARTESIAN_POINT('Origin',(0.,-0.04763,0.));
#10125=CARTESIAN_POINT('',(-0.841298510752802,-0.04763,-0.504455939115715));
#10126=CARTESIAN_POINT('Origin',(0.,-0.04763,0.));
#10127=CARTESIAN_POINT('Origin',(-0.707106781186547,-0.04763,-0.707106781186548));
#10128=CARTESIAN_POINT('Origin',(-0.707106781186547,0.,-0.707106781186548));
#10129=CARTESIAN_POINT('',(-0.504455939115715,-0.04763,-0.841298510752802));
#10130=CARTESIAN_POINT('Ctrl Pts',(-0.504455939115715,-0.04763,-0.841298510752802));
#10131=CARTESIAN_POINT('Ctrl Pts',(-0.508899795931835,-0.0740444353928835,
-0.838633903678357));
#10132=CARTESIAN_POINT('Ctrl Pts',(-0.517157748491652,-0.0999305678883309,
-0.833661031856294));
#10133=CARTESIAN_POINT('Ctrl Pts',(-0.537715343527944,-0.142345102874864,
-0.820511285096538));
#10134=CARTESIAN_POINT('Ctrl Pts',(-0.548874290046456,-0.159766064500479,
-0.813159949759));
#10135=CARTESIAN_POINT('Ctrl Pts',(-0.573915184558107,-0.190326085855194,
-0.795684265985089));
#10136=CARTESIAN_POINT('Ctrl Pts',(-0.587792702767295,-0.203463743702801,
-0.78555112003688));
#10137=CARTESIAN_POINT('Ctrl Pts',(-0.615966552324775,-0.224161999508995,
-0.763642258217233));
#10138=CARTESIAN_POINT('Ctrl Pts',(-0.631684198665438,-0.232861760990032,
-0.750785745543687));
#10139=CARTESIAN_POINT('Ctrl Pts',(-0.663382628119203,-0.244251601209411,
-0.722929908501543));
#10140=CARTESIAN_POINT('Ctrl Pts',(-0.679352081686668,-0.246942143572133,
-0.707917883896095));
#10141=CARTESIAN_POINT('Ctrl Pts',(-0.707917883896095,-0.246942143572133,
-0.679352081686668));
#10142=CARTESIAN_POINT('Ctrl Pts',(-0.722929908501543,-0.244251601209411,
-0.663382628119203));
#10143=CARTESIAN_POINT('Ctrl Pts',(-0.750785745543687,-0.232861760990032,
-0.631684198665439));
#10144=CARTESIAN_POINT('Ctrl Pts',(-0.763642258217232,-0.224161999508995,
-0.615966552324775));
#10145=CARTESIAN_POINT('Ctrl Pts',(-0.78555112003688,-0.203463743702801,
-0.587792702767295));
#10146=CARTESIAN_POINT('Ctrl Pts',(-0.795684265985088,-0.190326085855194,
-0.573915184558107));
#10147=CARTESIAN_POINT('Ctrl Pts',(-0.813159949759,-0.15976606450048,-0.548874290046456));
#10148=CARTESIAN_POINT('Ctrl Pts',(-0.820511285096538,-0.142345102874864,
-0.537715343527944));
#10149=CARTESIAN_POINT('Ctrl Pts',(-0.833661031856294,-0.0999305678883311,
-0.517157748491652));
#10150=CARTESIAN_POINT('Ctrl Pts',(-0.838633903678357,-0.0740444353928836,
-0.508899795931835));
#10151=CARTESIAN_POINT('Ctrl Pts',(-0.841298510752801,-0.04763,-0.504455939115715));
#10152=CARTESIAN_POINT('Origin',(-0.707106781186547,-0.04763,-0.707106781186548));
#10153=CARTESIAN_POINT('Origin',(0.,-0.04763,0.));
#10154=CARTESIAN_POINT('',(-0.238183666596899,-0.04763,-0.951592097314));
#10155=CARTESIAN_POINT('Origin',(0.,-0.04763,0.));
#10156=CARTESIAN_POINT('Origin',(5.55111512312578E-17,-0.04763,-1.));
#10157=CARTESIAN_POINT('Origin',(5.55111512312578E-17,0.,-1.));
#10158=CARTESIAN_POINT('',(0.238183666596899,-0.04763,-0.951592097314));
#10159=CARTESIAN_POINT('Ctrl Pts',(0.238183666596899,-0.04763,-0.951592097314));
#10160=CARTESIAN_POINT('Ctrl Pts',(0.233157223576062,-0.0740444353928835,
-0.952850216871763));
#10161=CARTESIAN_POINT('Ctrl Pts',(0.223801617934946,-0.099930567888331,
-0.955173119738174));
#10162=CARTESIAN_POINT('Ctrl Pts',(0.199966927975188,-0.142345102874864,
-0.960411259488514));
#10163=CARTESIAN_POINT('Ctrl Pts',(0.1868781821531,-0.15976606450048,-0.963103647174702));
#10164=CARTESIAN_POINT('Ctrl Pts',(0.15681442133453,-0.190326085855194,
-0.968453058988463));
#10165=CARTESIAN_POINT('Ctrl Pts',(0.139836317888042,-0.203463743702801,
-0.971100730005489));
#10166=CARTESIAN_POINT('Ctrl Pts',(0.104422493053067,-0.224161999508995,
-0.975530745318961));
#10167=CARTESIAN_POINT('Ctrl Pts',(0.0842175114474173,-0.232861760990032,
-0.977553872336861));
#10168=CARTESIAN_POINT('Ctrl Pts',(0.0421062857595698,-0.244251601209411,
-0.980270995488453));
#10169=CARTESIAN_POINT('Ctrl Pts',(0.0201990724523194,-0.246942143572133,
-0.980948));
#10170=CARTESIAN_POINT('Ctrl Pts',(-0.0201990724523193,-0.246942143572133,
-0.980948));
#10171=CARTESIAN_POINT('Ctrl Pts',(-0.0421062857595697,-0.244251601209411,
-0.980270995488453));
#10172=CARTESIAN_POINT('Ctrl Pts',(-0.0842175114474171,-0.232861760990032,
-0.977553872336861));
#10173=CARTESIAN_POINT('Ctrl Pts',(-0.104422493053067,-0.224161999508995,
-0.975530745318961));
#10174=CARTESIAN_POINT('Ctrl Pts',(-0.139836317888042,-0.203463743702801,
-0.971100730005489));
#10175=CARTESIAN_POINT('Ctrl Pts',(-0.15681442133453,-0.190326085855194,
-0.968453058988463));
#10176=CARTESIAN_POINT('Ctrl Pts',(-0.1868781821531,-0.15976606450048,-0.963103647174702));
#10177=CARTESIAN_POINT('Ctrl Pts',(-0.199966927975188,-0.142345102874864,
-0.960411259488514));
#10178=CARTESIAN_POINT('Ctrl Pts',(-0.223801617934945,-0.099930567888331,
-0.955173119738174));
#10179=CARTESIAN_POINT('Ctrl Pts',(-0.233157223576062,-0.0740444353928835,
-0.952850216871763));
#10180=CARTESIAN_POINT('Ctrl Pts',(-0.238183666596899,-0.0476299999999999,
-0.951592097314));
#10181=CARTESIAN_POINT('Origin',(5.55111512312578E-17,-0.04763,-1.));
#10182=CARTESIAN_POINT('Origin',(0.,-0.04763,0.));
#10183=CARTESIAN_POINT('',(0.504455939115715,-0.04763,-0.841298510752802));
#10184=CARTESIAN_POINT('Origin',(0.,-0.04763,0.));
#10185=CARTESIAN_POINT('Origin',(0.707106781186548,-0.04763,-0.707106781186547));
#10186=CARTESIAN_POINT('Origin',(0.707106781186548,0.,-0.707106781186547));
#10187=CARTESIAN_POINT('',(0.841298510752802,-0.04763,-0.504455939115715));
#10188=CARTESIAN_POINT('Ctrl Pts',(0.841298510752802,-0.04763,-0.504455939115715));
#10189=CARTESIAN_POINT('Ctrl Pts',(0.838633903678357,-0.0740444353928835,
-0.508899795931835));
#10190=CARTESIAN_POINT('Ctrl Pts',(0.833661031856294,-0.0999305678883309,
-0.517157748491652));
#10191=CARTESIAN_POINT('Ctrl Pts',(0.820511285096538,-0.142345102874864,
-0.537715343527944));
#10192=CARTESIAN_POINT('Ctrl Pts',(0.813159949759,-0.159766064500479,-0.548874290046456));
#10193=CARTESIAN_POINT('Ctrl Pts',(0.795684265985088,-0.190326085855194,
-0.573915184558107));
#10194=CARTESIAN_POINT('Ctrl Pts',(0.78555112003688,-0.203463743702801,
-0.587792702767295));
#10195=CARTESIAN_POINT('Ctrl Pts',(0.763642258217233,-0.224161999508995,
-0.615966552324775));
#10196=CARTESIAN_POINT('Ctrl Pts',(0.750785745543687,-0.232861760990032,
-0.631684198665438));
#10197=CARTESIAN_POINT('Ctrl Pts',(0.722929908501543,-0.244251601209411,
-0.663382628119203));
#10198=CARTESIAN_POINT('Ctrl Pts',(0.707917883896095,-0.246942143572133,
-0.679352081686668));
#10199=CARTESIAN_POINT('Ctrl Pts',(0.679352081686668,-0.246942143572133,
-0.707917883896095));
#10200=CARTESIAN_POINT('Ctrl Pts',(0.663382628119203,-0.244251601209411,
-0.722929908501543));
#10201=CARTESIAN_POINT('Ctrl Pts',(0.631684198665438,-0.232861760990032,
-0.750785745543687));
#10202=CARTESIAN_POINT('Ctrl Pts',(0.615966552324775,-0.224161999508995,
-0.763642258217232));
#10203=CARTESIAN_POINT('Ctrl Pts',(0.587792702767295,-0.203463743702801,
-0.78555112003688));
#10204=CARTESIAN_POINT('Ctrl Pts',(0.573915184558107,-0.190326085855194,
-0.795684265985088));
#10205=CARTESIAN_POINT('Ctrl Pts',(0.548874290046456,-0.159766064500479,
-0.813159949759));
#10206=CARTESIAN_POINT('Ctrl Pts',(0.537715343527944,-0.142345102874864,
-0.820511285096538));
#10207=CARTESIAN_POINT('Ctrl Pts',(0.517157748491652,-0.099930567888331,
-0.833661031856294));
#10208=CARTESIAN_POINT('Ctrl Pts',(0.508899795931835,-0.0740444353928835,
-0.838633903678357));
#10209=CARTESIAN_POINT('Ctrl Pts',(0.504455939115715,-0.04763,-0.841298510752801));
#10210=CARTESIAN_POINT('Origin',(0.707106781186548,-0.04763,-0.707106781186547));
#10211=CARTESIAN_POINT('Origin',(0.,-0.166705,0.));
#10212=CARTESIAN_POINT('',(-0.980948,-0.28578,1.20131482833E-16));
#10213=CARTESIAN_POINT('Origin',(0.,-0.28578,0.));
#10214=CARTESIAN_POINT('',(-0.980948,-0.166705,1.20131482833E-16));
#10215=CARTESIAN_POINT('',(0.951592097314,-0.04763,0.238183666596899));
#10216=CARTESIAN_POINT('Origin',(0.,-0.04763,0.));
#10217=CARTESIAN_POINT('',(0.951592097314,-0.04763,-0.238183666596899));
#10218=CARTESIAN_POINT('Ctrl Pts',(0.951592097314,-0.04763,0.238183666596899));
#10219=CARTESIAN_POINT('Ctrl Pts',(0.952850216871763,-0.0740444353928835,
0.233157223576062));
#10220=CARTESIAN_POINT('Ctrl Pts',(0.955173119738174,-0.099930567888331,
0.223801617934945));
#10221=CARTESIAN_POINT('Ctrl Pts',(0.960411259488514,-0.142345102874864,
0.199966927975188));
#10222=CARTESIAN_POINT('Ctrl Pts',(0.963103647174702,-0.15976606450048,
0.1868781821531));
#10223=CARTESIAN_POINT('Ctrl Pts',(0.968453058988463,-0.190326085855194,
0.15681442133453));
#10224=CARTESIAN_POINT('Ctrl Pts',(0.971100730005489,-0.203463743702801,
0.139836317888042));
#10225=CARTESIAN_POINT('Ctrl Pts',(0.975530745318961,-0.224161999508995,
0.104422493053067));
#10226=CARTESIAN_POINT('Ctrl Pts',(0.977553872336861,-0.232861760990032,
0.0842175114474172));
#10227=CARTESIAN_POINT('Ctrl Pts',(0.980270995488453,-0.244251601209411,
0.0421062857595697));
#10228=CARTESIAN_POINT('Ctrl Pts',(0.980948,-0.246942143572133,0.0201990724523194));
#10229=CARTESIAN_POINT('Ctrl Pts',(0.980948,-0.246942143572133,-0.0201990724523194));
#10230=CARTESIAN_POINT('Ctrl Pts',(0.980270995488453,-0.244251601209411,
-0.0421062857595697));
#10231=CARTESIAN_POINT('Ctrl Pts',(0.977553872336861,-0.232861760990032,
-0.0842175114474172));
#10232=CARTESIAN_POINT('Ctrl Pts',(0.975530745318961,-0.224161999508995,
-0.104422493053067));
#10233=CARTESIAN_POINT('Ctrl Pts',(0.971100730005489,-0.203463743702801,
-0.139836317888042));
#10234=CARTESIAN_POINT('Ctrl Pts',(0.968453058988463,-0.190326085855194,
-0.15681442133453));
#10235=CARTESIAN_POINT('Ctrl Pts',(0.963103647174702,-0.15976606450048,
-0.1868781821531));
#10236=CARTESIAN_POINT('Ctrl Pts',(0.960411259488514,-0.142345102874864,
-0.199966927975188));
#10237=CARTESIAN_POINT('Ctrl Pts',(0.955173119738174,-0.099930567888331,
-0.223801617934945));
#10238=CARTESIAN_POINT('Ctrl Pts',(0.952850216871763,-0.0740444353928835,
-0.233157223576062));
#10239=CARTESIAN_POINT('Ctrl Pts',(0.951592097314,-0.0476299999999999,-0.238183666596899));
#10240=CARTESIAN_POINT('Origin',(0.,-0.04763,0.));
#10241=CARTESIAN_POINT('Origin',(0.,-0.04763,0.));
#10242=CARTESIAN_POINT('Origin',(1.,-0.04763,0.));
#10243=CARTESIAN_POINT('Origin',(1.,0.,0.));
#10244=CARTESIAN_POINT('Origin',(1.,-0.04763,0.));
#10245=CARTESIAN_POINT('Origin',(0.,-0.28578,0.));
#10246=CARTESIAN_POINT('Origin',(0.,-0.04763,0.));
#10247=CARTESIAN_POINT('',(0.,0.,0.));
#10248=CARTESIAN_POINT('Origin',(1.013815,0.445,0.));
#10249=CARTESIAN_POINT('',(-1.013815,0.445,-1.24156529467757E-16));
#10250=CARTESIAN_POINT('Origin',(0.,0.445,0.));
#10251=CARTESIAN_POINT('',(-0.991185,0.445,-1.21385153761287E-16));
#10252=CARTESIAN_POINT('Origin',(0.,0.445,0.));
#10253=CARTESIAN_POINT('Origin',(0.,0.4075,0.));
#10254=CARTESIAN_POINT('',(-1.013815,0.37,-1.24156529467757E-16));
#10255=CARTESIAN_POINT('Origin',(0.,0.37,0.));
#10256=CARTESIAN_POINT('',(-1.013815,0.4075,-1.24156529467757E-16));
#10257=CARTESIAN_POINT('Origin',(0.991185,0.37,0.));
#10258=CARTESIAN_POINT('',(-0.991185,0.37,-1.21385153761287E-16));
#10259=CARTESIAN_POINT('Origin',(0.,0.37,0.));
#10260=CARTESIAN_POINT('Origin',(0.,0.4075,0.));
#10261=CARTESIAN_POINT('',(-0.991185,0.4075,-1.21385153761287E-16));
#10262=CARTESIAN_POINT('Origin',(1.013815,-0.37,0.));
#10263=CARTESIAN_POINT('',(-1.013815,-0.37,-1.24156529467757E-16));
#10264=CARTESIAN_POINT('Origin',(0.,-0.37,0.));
#10265=CARTESIAN_POINT('',(-0.991185,-0.37,-1.21385153761287E-16));
#10266=CARTESIAN_POINT('Origin',(0.,-0.37,0.));
#10267=CARTESIAN_POINT('Origin',(0.,-0.4075,0.));
#10268=CARTESIAN_POINT('',(-1.013815,-0.445,-1.24156529467757E-16));
#10269=CARTESIAN_POINT('Origin',(0.,-0.445,0.));
#10270=CARTESIAN_POINT('',(-1.013815,-0.4075,-1.24156529467757E-16));
#10271=CARTESIAN_POINT('Origin',(0.991185,-0.445,0.));
#10272=CARTESIAN_POINT('',(-0.991185,-0.445,-1.21385153761287E-16));
#10273=CARTESIAN_POINT('Origin',(0.,-0.445,0.));
#10274=CARTESIAN_POINT('Origin',(0.,-0.4075,0.));
#10275=CARTESIAN_POINT('',(-0.991185,-0.4075,-1.21385153761287E-16));
#10276=CARTESIAN_POINT('',(0.,0.,0.));
#10277=CARTESIAN_POINT('',(0.,0.,0.));
#10278=CARTESIAN_POINT('',(0.,0.,0.));
#10279=CARTESIAN_POINT('',(0.,0.,0.));
#10280=CARTESIAN_POINT('',(0.,0.,0.));
#10281=CARTESIAN_POINT('',(0.,0.,0.));
#10282=CARTESIAN_POINT('Origin',(0.3,0.4,0.));
#10283=CARTESIAN_POINT('',(-0.3,0.4,-3.67394039744206E-17));
#10284=CARTESIAN_POINT('Origin',(0.,0.4,0.));
#10285=CARTESIAN_POINT('Origin',(0.,0.375,0.));
#10286=CARTESIAN_POINT('',(-0.35,0.35,-4.28626379701573E-17));
#10287=CARTESIAN_POINT('Origin',(0.,0.35,0.));
#10288=CARTESIAN_POINT('',(-0.325,0.375,-3.9801020972289E-17));
#10289=CARTESIAN_POINT('Origin',(0.,0.19,0.));
#10290=CARTESIAN_POINT('',(-0.35,0.03,-4.28626379701574E-17));
#10291=CARTESIAN_POINT('Origin',(0.,0.03,0.));
#10292=CARTESIAN_POINT('',(-0.35,0.19,-4.28626379701574E-17));
#10293=CARTESIAN_POINT('Origin',(0.,0.0149999999999999,0.));
#10294=CARTESIAN_POINT('',(-0.32,-3.29597460435593E-17,-3.91886975727153E-17));
#10295=CARTESIAN_POINT('Origin',(0.,0.,0.));
#10296=CARTESIAN_POINT('',(-0.335,0.0149999999999999,-4.10256677714363E-17));
#10297=CARTESIAN_POINT('Origin',(0.22,0.,0.));
#10298=CARTESIAN_POINT('',(-0.22,-6.93889390390723E-18,-2.69422295812418E-17));
#10299=CARTESIAN_POINT('Origin',(0.,0.,0.));
#10300=CARTESIAN_POINT('Origin',(0.,-0.02,0.));
#10301=CARTESIAN_POINT('',(-0.1954,-0.0492,2.39295984553393E-17));
#10302=CARTESIAN_POINT('Origin',(0.,-0.0492,0.));
#10303=CARTESIAN_POINT('',(-0.21,-0.02,-2.57175827820944E-17));
#10304=CARTESIAN_POINT('Origin',(0.,-0.8,0.));
#10305=CARTESIAN_POINT('',(-0.1954,-1.5646,2.39295984553393E-17));
#10306=CARTESIAN_POINT('Origin',(0.,-1.5646,0.));
#10307=CARTESIAN_POINT('',(-0.1954,-0.8,-2.39295984553393E-17));
#10308=CARTESIAN_POINT('Origin',(0.,-1.58,0.));
#10309=CARTESIAN_POINT('',(-0.16,-1.6,-1.95943487863577E-17));
#10310=CARTESIAN_POINT('Origin',(0.,-1.6,0.));
#10311=CARTESIAN_POINT('',(-0.18,-1.58,-2.20436423846524E-17));
#10312=CARTESIAN_POINT('Origin',(0.,-1.6,0.));
#10313=CARTESIAN_POINT('Origin',(0.0866025403784439,-0.4,-0.15));
#10314=CARTESIAN_POINT('',(0.173205080756888,-0.4,0.));
#10315=CARTESIAN_POINT('',(0.0866025403784439,-0.4,-0.15));
#10316=CARTESIAN_POINT('',(0.173205080756888,-0.4,0.));
#10317=CARTESIAN_POINT('',(0.0866025403784439,-0.64,-0.15));
#10318=CARTESIAN_POINT('',(0.0866025403784439,-0.4,-0.15));
#10319=CARTESIAN_POINT('',(0.173205080756888,-0.64,0.));
#10320=CARTESIAN_POINT('',(0.173205080756888,-0.64,0.));
#10321=CARTESIAN_POINT('',(0.173205080756888,-0.4,0.));
#10322=CARTESIAN_POINT('Origin',(-0.0866025403784438,-0.4,-0.15));
#10323=CARTESIAN_POINT('',(-0.0866025403784438,-0.4,-0.15));
#10324=CARTESIAN_POINT('',(0.0866025403784439,-0.4,-0.15));
#10325=CARTESIAN_POINT('',(-0.0866025403784438,-0.64,-0.15));
#10326=CARTESIAN_POINT('',(-0.0866025403784438,-0.4,-0.15));
#10327=CARTESIAN_POINT('',(0.0866025403784439,-0.64,-0.15));
#10328=CARTESIAN_POINT('Origin',(-0.173205080756888,-0.4,-2.77555756156289E-17));
#10329=CARTESIAN_POINT('',(-0.173205080756888,-0.4,-2.12115047744981E-17));
#10330=CARTESIAN_POINT('',(-0.0866025403784438,-0.4,-0.15));
#10331=CARTESIAN_POINT('',(-0.173205080756888,-0.64,-2.77555756156289E-17));
#10332=CARTESIAN_POINT('',(-0.173205080756888,-0.4,-2.12115047744981E-17));
#10333=CARTESIAN_POINT('',(-0.0866025403784438,-0.64,-0.15));
#10334=CARTESIAN_POINT('Origin',(-0.0866025403784439,-0.4,0.15));
#10335=CARTESIAN_POINT('',(-0.0866025403784439,-0.4,0.15));
#10336=CARTESIAN_POINT('',(-0.173205080756888,-0.4,-2.12115047744981E-17));
#10337=CARTESIAN_POINT('',(-0.0866025403784439,-0.64,0.15));
#10338=CARTESIAN_POINT('',(-0.0866025403784439,-0.4,0.15));
#10339=CARTESIAN_POINT('',(-0.173205080756888,-0.64,-2.12115047744981E-17));
#10340=CARTESIAN_POINT('Origin',(0.0866025403784439,-0.4,0.15));
#10341=CARTESIAN_POINT('',(0.0866025403784439,-0.4,0.15));
#10342=CARTESIAN_POINT('',(-0.0866025403784439,-0.4,0.15));
#10343=CARTESIAN_POINT('',(0.0866025403784439,-0.64,0.15));
#10344=CARTESIAN_POINT('',(0.0866025403784439,-0.4,0.15));
#10345=CARTESIAN_POINT('',(-0.0866025403784439,-0.64,0.15));
#10346=CARTESIAN_POINT('Origin',(0.173205080756888,-0.4,0.));
#10347=CARTESIAN_POINT('',(0.0866025403784439,-0.4,0.15));
#10348=CARTESIAN_POINT('',(0.0866025403784439,-0.64,0.15));
#10349=CARTESIAN_POINT('Origin',(0.,-0.4,-2.77555756156289E-17));
#10350=CARTESIAN_POINT('Origin',(0.,-0.64,-2.77555756156289E-17));
#10351=CARTESIAN_POINT('',(0.,0.,0.));
#10352=CARTESIAN_POINT('',(0.,0.,0.));
#10353=CARTESIAN_POINT('',(0.,0.,0.));
#10354=CARTESIAN_POINT('',(0.,0.,0.));
#10355=CARTESIAN_POINT('',(0.,0.,0.));
#10356=CARTESIAN_POINT('',(0.,0.,0.));
#10357=CARTESIAN_POINT('',(0.,0.,0.));
#10358=CARTESIAN_POINT('',(-3.3,1.,1.8));
#10359=CARTESIAN_POINT('',(-3.3,1.,1.96));
#10360=CARTESIAN_POINT('',(-3.3,3.,1.8));
#10361=CARTESIAN_POINT('',(-3.3,3.,1.96));
#10362=CARTESIAN_POINT('',(3.3,1.,1.8));
#10363=CARTESIAN_POINT('',(3.3,1.,1.96));
#10364=CARTESIAN_POINT('',(3.3,3.,1.8));
#10365=CARTESIAN_POINT('',(3.3,3.,1.96));
#10366=CARTESIAN_POINT('',(0.,0.,10.));
#10367=CARTESIAN_POINT('',(0.,4.,10.));
#10368=CARTESIAN_POINT('',(1.4142135623731,-0.9,11.4142135623731));
#10369=CARTESIAN_POINT('',(-1.41421356237309,-0.9,11.4142135623731));
#10370=CARTESIAN_POINT('',(-1.4142135623731,-0.9,8.5857864376269));
#10371=CARTESIAN_POINT('',(1.41421356237309,-0.9,8.5857864376269));
#10372=CARTESIAN_POINT('',(1.4142135623731,4.9,11.4142135623731));
#10373=CARTESIAN_POINT('',(-1.41421356237309,4.9,11.4142135623731));
#10374=CARTESIAN_POINT('',(-1.4142135623731,4.9,8.5857864376269));
#10375=CARTESIAN_POINT('',(1.41421356237309,4.9,8.5857864376269));
#10376=CARTESIAN_POINT('',(0.,0.,0.));
#10377=CARTESIAN_POINT('',(0.,0.,0.));
#10378=CARTESIAN_POINT('',(0.,0.,0.));
#10379=CARTESIAN_POINT('',(0.,0.,0.));
#10380=CARTESIAN_POINT('',(0.,0.,0.));
#10381=CARTESIAN_POINT('',(0.,0.,0.));
#10382=CARTESIAN_POINT('',(0.,0.,0.));
#10383=CARTESIAN_POINT('',(0.,-2.5,9.65));
#10384=CARTESIAN_POINT('',(0.,-2.,11.4));
#10385=CARTESIAN_POINT('',(0.,5.3,11.4));
#10386=CARTESIAN_POINT('',(5.3,-3.4,10.));
#10387=CARTESIAN_POINT('',(7.7,-3.4,10.));
#10388=CARTESIAN_POINT('',(6.5,-5.,10.));
#10389=CARTESIAN_POINT('',(6.5,-6.2,10.));
#10390=CARTESIAN_POINT('',(0.,0.,0.));
#10391=CARTESIAN_POINT('',(0.,0.,0.));
#10392=CARTESIAN_POINT('Origin',(6.5,-5.45,10.));
#10393=CARTESIAN_POINT('',(5.,-5.45,10.));
#10394=CARTESIAN_POINT('Origin',(6.5,-5.45,10.));
#10395=CARTESIAN_POINT('',(5.,-4.55,10.));
#10396=CARTESIAN_POINT('',(5.,-5.45,10.));
#10397=CARTESIAN_POINT('Origin',(6.5,-4.55,10.));
#10398=CARTESIAN_POINT('Origin',(6.5,-5.45,10.));
#10399=CARTESIAN_POINT('',(5.59,-5.45,10.));
#10400=CARTESIAN_POINT('Origin',(6.5,-5.45,10.));
#10401=CARTESIAN_POINT('Origin',(6.5,-10.,10.));
#10402=CARTESIAN_POINT('',(5.59,-10.,10.));
#10403=CARTESIAN_POINT('',(5.59,-10.,10.));
#10404=CARTESIAN_POINT('Origin',(6.5,-10.,10.));
#10405=CARTESIAN_POINT('Origin',(6.5,-10.,10.));
#10406=CARTESIAN_POINT('',(4.7,-4.55,10.));
#10407=CARTESIAN_POINT('Origin',(6.5,-4.55,10.));
#10408=CARTESIAN_POINT('',(4.7,-10.,10.));
#10409=CARTESIAN_POINT('',(4.7,-10.,10.));
#10410=CARTESIAN_POINT('Origin',(6.5,-10.,10.));
#10411=CARTESIAN_POINT('Origin',(6.5,-4.55,10.));
#10412=CARTESIAN_POINT('Origin',(6.5,-10.,10.));
#10413=CARTESIAN_POINT('',(0.,0.,0.));
#10414=CARTESIAN_POINT('Origin',(6.5,-4.55,10.));
#10415=CARTESIAN_POINT('',(5.59,-4.25,10.));
#10416=CARTESIAN_POINT('Origin',(6.5,-4.25,10.));
#10417=CARTESIAN_POINT('',(5.59,-4.55,10.));
#10418=CARTESIAN_POINT('',(5.59,-4.55,10.));
#10419=CARTESIAN_POINT('Origin',(6.5,-4.55,10.));
#10420=CARTESIAN_POINT('Origin',(6.5,-4.55,10.));
#10421=CARTESIAN_POINT('',(4.7,-4.25,10.));
#10422=CARTESIAN_POINT('Origin',(6.5,-4.25,10.));
#10423=CARTESIAN_POINT('',(4.7,-4.55,10.));
#10424=CARTESIAN_POINT('',(4.7,-4.55,10.));
#10425=CARTESIAN_POINT('Origin',(6.5,-4.55,10.));
#10426=CARTESIAN_POINT('Origin',(6.5,-4.25,10.));
#10427=CARTESIAN_POINT('Origin',(6.5,-4.55,10.));
#10428=CARTESIAN_POINT('',(0.,0.,0.));
#10429=CARTESIAN_POINT('',(0.,0.,0.));
#10430=CARTESIAN_POINT('',(0.,0.,0.));
#10431=CARTESIAN_POINT('',(0.,0.,0.));
#10432=CARTESIAN_POINT('',(0.,0.,0.));
#10433=UNCERTAINTY_MEASURE_WITH_UNIT(LENGTH_MEASURE(0.001),#10511,
'DISTANCE_ACCURACY_VALUE',
'Maximum model space distance between geometric entities at asserted c
onnectivities');
#10434=UNCERTAINTY_MEASURE_WITH_UNIT(LENGTH_MEASURE(0.001),#10511,
'DISTANCE_ACCURACY_VALUE',
'Maximum model space distance between geometric entities at asserted c
onnectivities');
#10435=UNCERTAINTY_MEASURE_WITH_UNIT(LENGTH_MEASURE(0.001),#10511,
'DISTANCE_ACCURACY_VALUE',
'Maximum model space distance between geometric entities at asserted c
onnectivities');
#10436=UNCERTAINTY_MEASURE_WITH_UNIT(LENGTH_MEASURE(0.001),#10511,
'DISTANCE_ACCURACY_VALUE',
'Maximum model space distance between geometric entities at asserted c
onnectivities');
#10437=UNCERTAINTY_MEASURE_WITH_UNIT(LENGTH_MEASURE(0.001),#10511,
'DISTANCE_ACCURACY_VALUE',
'Maximum model space distance between geometric entities at asserted c
onnectivities');
#10438=UNCERTAINTY_MEASURE_WITH_UNIT(LENGTH_MEASURE(0.001),#10511,
'DISTANCE_ACCURACY_VALUE',
'Maximum model space distance between geometric entities at asserted c
onnectivities');
#10439=UNCERTAINTY_MEASURE_WITH_UNIT(LENGTH_MEASURE(0.001),#10511,
'DISTANCE_ACCURACY_VALUE',
'Maximum model space distance between geometric entities at asserted c
onnectivities');
#10440=UNCERTAINTY_MEASURE_WITH_UNIT(LENGTH_MEASURE(0.001),#10511,
'DISTANCE_ACCURACY_VALUE',
'Maximum model space distance between geometric entities at asserted c
onnectivities');
#10441=UNCERTAINTY_MEASURE_WITH_UNIT(LENGTH_MEASURE(0.001),#10511,
'DISTANCE_ACCURACY_VALUE',
'Maximum model space distance between geometric entities at asserted c
onnectivities');
#10442=UNCERTAINTY_MEASURE_WITH_UNIT(LENGTH_MEASURE(0.001),#10511,
'DISTANCE_ACCURACY_VALUE',
'Maximum model space distance between geometric entities at asserted c
onnectivities');
#10443=UNCERTAINTY_MEASURE_WITH_UNIT(LENGTH_MEASURE(0.001),#10511,
'DISTANCE_ACCURACY_VALUE',
'Maximum model space distance between geometric entities at asserted c
onnectivities');
#10444=UNCERTAINTY_MEASURE_WITH_UNIT(LENGTH_MEASURE(0.001),#10511,
'DISTANCE_ACCURACY_VALUE',
'Maximum model space distance between geometric entities at asserted c
onnectivities');
#10445=UNCERTAINTY_MEASURE_WITH_UNIT(LENGTH_MEASURE(0.001),#10511,
'DISTANCE_ACCURACY_VALUE',
'Maximum model space distance between geometric entities at asserted c
onnectivities');
#10446=UNCERTAINTY_MEASURE_WITH_UNIT(LENGTH_MEASURE(0.001),#10511,
'DISTANCE_ACCURACY_VALUE',
'Maximum model space distance between geometric entities at asserted c
onnectivities');
#10447=UNCERTAINTY_MEASURE_WITH_UNIT(LENGTH_MEASURE(0.001),#10511,
'DISTANCE_ACCURACY_VALUE',
'Maximum model space distance between geometric entities at asserted c
onnectivities');
#10448=UNCERTAINTY_MEASURE_WITH_UNIT(LENGTH_MEASURE(0.001),#10511,
'DISTANCE_ACCURACY_VALUE',
'Maximum model space distance between geometric entities at asserted c
onnectivities');
#10449=UNCERTAINTY_MEASURE_WITH_UNIT(LENGTH_MEASURE(0.001),#10511,
'DISTANCE_ACCURACY_VALUE',
'Maximum model space distance between geometric entities at asserted c
onnectivities');
#10450=UNCERTAINTY_MEASURE_WITH_UNIT(LENGTH_MEASURE(0.001),#10511,
'DISTANCE_ACCURACY_VALUE',
'Maximum model space distance between geometric entities at asserted c
onnectivities');
#10451=UNCERTAINTY_MEASURE_WITH_UNIT(LENGTH_MEASURE(0.001),#10511,
'DISTANCE_ACCURACY_VALUE',
'Maximum model space distance between geometric entities at asserted c
onnectivities');
#10452=UNCERTAINTY_MEASURE_WITH_UNIT(LENGTH_MEASURE(0.001),#10511,
'DISTANCE_ACCURACY_VALUE',
'Maximum model space distance between geometric entities at asserted c
onnectivities');
#10453=UNCERTAINTY_MEASURE_WITH_UNIT(LENGTH_MEASURE(0.001),#10511,
'DISTANCE_ACCURACY_VALUE',
'Maximum model space distance between geometric entities at asserted c
onnectivities');
#10454=UNCERTAINTY_MEASURE_WITH_UNIT(LENGTH_MEASURE(0.001),#10511,
'DISTANCE_ACCURACY_VALUE',
'Maximum model space distance between geometric entities at asserted c
onnectivities');
#10455=UNCERTAINTY_MEASURE_WITH_UNIT(LENGTH_MEASURE(0.001),#10511,
'DISTANCE_ACCURACY_VALUE',
'Maximum model space distance between geometric entities at asserted c
onnectivities');
#10456=UNCERTAINTY_MEASURE_WITH_UNIT(LENGTH_MEASURE(0.001),#10511,
'DISTANCE_ACCURACY_VALUE',
'Maximum model space distance between geometric entities at asserted c
onnectivities');
#10457=UNCERTAINTY_MEASURE_WITH_UNIT(LENGTH_MEASURE(0.001),#10511,
'DISTANCE_ACCURACY_VALUE',
'Maximum model space distance between geometric entities at asserted c
onnectivities');
#10458=UNCERTAINTY_MEASURE_WITH_UNIT(LENGTH_MEASURE(0.001),#10511,
'DISTANCE_ACCURACY_VALUE',
'Maximum model space distance between geometric entities at asserted c
onnectivities');
#10459=UNCERTAINTY_MEASURE_WITH_UNIT(LENGTH_MEASURE(0.001),#10511,
'DISTANCE_ACCURACY_VALUE',
'Maximum model space distance between geometric entities at asserted c
onnectivities');
#10460=UNCERTAINTY_MEASURE_WITH_UNIT(LENGTH_MEASURE(0.001),#10511,
'DISTANCE_ACCURACY_VALUE',
'Maximum model space distance between geometric entities at asserted c
onnectivities');
#10461=UNCERTAINTY_MEASURE_WITH_UNIT(LENGTH_MEASURE(0.001),#10511,
'DISTANCE_ACCURACY_VALUE',
'Maximum model space distance between geometric entities at asserted c
onnectivities');
#10462=UNCERTAINTY_MEASURE_WITH_UNIT(LENGTH_MEASURE(0.001),#10511,
'DISTANCE_ACCURACY_VALUE',
'Maximum model space distance between geometric entities at asserted c
onnectivities');
#10463=UNCERTAINTY_MEASURE_WITH_UNIT(LENGTH_MEASURE(0.001),#10511,
'DISTANCE_ACCURACY_VALUE',
'Maximum model space distance between geometric entities at asserted c
onnectivities');
#10464=UNCERTAINTY_MEASURE_WITH_UNIT(LENGTH_MEASURE(0.001),#10511,
'DISTANCE_ACCURACY_VALUE',
'Maximum model space distance between geometric entities at asserted c
onnectivities');
#10465=UNCERTAINTY_MEASURE_WITH_UNIT(LENGTH_MEASURE(0.001),#10511,
'DISTANCE_ACCURACY_VALUE',
'Maximum model space distance between geometric entities at asserted c
onnectivities');
#10466=UNCERTAINTY_MEASURE_WITH_UNIT(LENGTH_MEASURE(0.001),#10511,
'DISTANCE_ACCURACY_VALUE',
'Maximum model space distance between geometric entities at asserted c
onnectivities');
#10467=UNCERTAINTY_MEASURE_WITH_UNIT(LENGTH_MEASURE(0.001),#10511,
'DISTANCE_ACCURACY_VALUE',
'Maximum model space distance between geometric entities at asserted c
onnectivities');
#10468=UNCERTAINTY_MEASURE_WITH_UNIT(LENGTH_MEASURE(0.001),#10511,
'DISTANCE_ACCURACY_VALUE',
'Maximum model space distance between geometric entities at asserted c
onnectivities');
#10469=UNCERTAINTY_MEASURE_WITH_UNIT(LENGTH_MEASURE(0.001),#10511,
'DISTANCE_ACCURACY_VALUE',
'Maximum model space distance between geometric entities at asserted c
onnectivities');
#10470=UNCERTAINTY_MEASURE_WITH_UNIT(LENGTH_MEASURE(0.001),#10511,
'DISTANCE_ACCURACY_VALUE',
'Maximum model space distance between geometric entities at asserted c
onnectivities');
#10471=UNCERTAINTY_MEASURE_WITH_UNIT(LENGTH_MEASURE(0.001),#10511,
'DISTANCE_ACCURACY_VALUE',
'Maximum model space distance between geometric entities at asserted c
onnectivities');
#10472=(
GEOMETRIC_REPRESENTATION_CONTEXT(3)
GLOBAL_UNCERTAINTY_ASSIGNED_CONTEXT((#10433))
GLOBAL_UNIT_ASSIGNED_CONTEXT((#10511,#10513,#10514))
REPRESENTATION_CONTEXT('','3D')
);
#10473=(
GEOMETRIC_REPRESENTATION_CONTEXT(3)
GLOBAL_UNCERTAINTY_ASSIGNED_CONTEXT((#10434))
GLOBAL_UNIT_ASSIGNED_CONTEXT((#10511,#10513,#10514))
REPRESENTATION_CONTEXT('','3D')
);
#10474=(
GEOMETRIC_REPRESENTATION_CONTEXT(3)
GLOBAL_UNCERTAINTY_ASSIGNED_CONTEXT((#10435))
GLOBAL_UNIT_ASSIGNED_CONTEXT((#10511,#10513,#10514))
REPRESENTATION_CONTEXT('','3D')
);
#10475=(
GEOMETRIC_REPRESENTATION_CONTEXT(3)
GLOBAL_UNCERTAINTY_ASSIGNED_CONTEXT((#10436))
GLOBAL_UNIT_ASSIGNED_CONTEXT((#10511,#10513,#10514))
REPRESENTATION_CONTEXT('','3D')
);
#10476=(
GEOMETRIC_REPRESENTATION_CONTEXT(3)
GLOBAL_UNCERTAINTY_ASSIGNED_CONTEXT((#10437))
GLOBAL_UNIT_ASSIGNED_CONTEXT((#10511,#10513,#10514))
REPRESENTATION_CONTEXT('','3D')
);
#10477=(
GEOMETRIC_REPRESENTATION_CONTEXT(3)
GLOBAL_UNCERTAINTY_ASSIGNED_CONTEXT((#10438))
GLOBAL_UNIT_ASSIGNED_CONTEXT((#10511,#10513,#10514))
REPRESENTATION_CONTEXT('','3D')
);
#10478=(
GEOMETRIC_REPRESENTATION_CONTEXT(3)
GLOBAL_UNCERTAINTY_ASSIGNED_CONTEXT((#10439))
GLOBAL_UNIT_ASSIGNED_CONTEXT((#10511,#10513,#10514))
REPRESENTATION_CONTEXT('','3D')
);
#10479=(
GEOMETRIC_REPRESENTATION_CONTEXT(3)
GLOBAL_UNCERTAINTY_ASSIGNED_CONTEXT((#10440))
GLOBAL_UNIT_ASSIGNED_CONTEXT((#10511,#10513,#10514))
REPRESENTATION_CONTEXT('','3D')
);
#10480=(
GEOMETRIC_REPRESENTATION_CONTEXT(3)
GLOBAL_UNCERTAINTY_ASSIGNED_CONTEXT((#10441))
GLOBAL_UNIT_ASSIGNED_CONTEXT((#10511,#10513,#10514))
REPRESENTATION_CONTEXT('','3D')
);
#10481=(
GEOMETRIC_REPRESENTATION_CONTEXT(3)
GLOBAL_UNCERTAINTY_ASSIGNED_CONTEXT((#10442))
GLOBAL_UNIT_ASSIGNED_CONTEXT((#10511,#10513,#10514))
REPRESENTATION_CONTEXT('','3D')
);
#10482=(
GEOMETRIC_REPRESENTATION_CONTEXT(3)
GLOBAL_UNCERTAINTY_ASSIGNED_CONTEXT((#10443))
GLOBAL_UNIT_ASSIGNED_CONTEXT((#10511,#10513,#10514))
REPRESENTATION_CONTEXT('','3D')
);
#10483=(
GEOMETRIC_REPRESENTATION_CONTEXT(3)
GLOBAL_UNCERTAINTY_ASSIGNED_CONTEXT((#10444))
GLOBAL_UNIT_ASSIGNED_CONTEXT((#10511,#10513,#10514))
REPRESENTATION_CONTEXT('','3D')
);
#10484=(
GEOMETRIC_REPRESENTATION_CONTEXT(3)
GLOBAL_UNCERTAINTY_ASSIGNED_CONTEXT((#10445))
GLOBAL_UNIT_ASSIGNED_CONTEXT((#10511,#10513,#10514))
REPRESENTATION_CONTEXT('','3D')
);
#10485=(
GEOMETRIC_REPRESENTATION_CONTEXT(3)
GLOBAL_UNCERTAINTY_ASSIGNED_CONTEXT((#10446))
GLOBAL_UNIT_ASSIGNED_CONTEXT((#10511,#10513,#10514))
REPRESENTATION_CONTEXT('','3D')
);
#10486=(
GEOMETRIC_REPRESENTATION_CONTEXT(3)
GLOBAL_UNCERTAINTY_ASSIGNED_CONTEXT((#10447))
GLOBAL_UNIT_ASSIGNED_CONTEXT((#10511,#10513,#10514))
REPRESENTATION_CONTEXT('','3D')
);
#10487=(
GEOMETRIC_REPRESENTATION_CONTEXT(3)
GLOBAL_UNCERTAINTY_ASSIGNED_CONTEXT((#10448))
GLOBAL_UNIT_ASSIGNED_CONTEXT((#10511,#10513,#10514))
REPRESENTATION_CONTEXT('','3D')
);
#10488=(
GEOMETRIC_REPRESENTATION_CONTEXT(3)
GLOBAL_UNCERTAINTY_ASSIGNED_CONTEXT((#10449))
GLOBAL_UNIT_ASSIGNED_CONTEXT((#10511,#10513,#10514))
REPRESENTATION_CONTEXT('','3D')
);
#10489=(
GEOMETRIC_REPRESENTATION_CONTEXT(3)
GLOBAL_UNCERTAINTY_ASSIGNED_CONTEXT((#10450))
GLOBAL_UNIT_ASSIGNED_CONTEXT((#10511,#10513,#10514))
REPRESENTATION_CONTEXT('','3D')
);
#10490=(
GEOMETRIC_REPRESENTATION_CONTEXT(3)
GLOBAL_UNCERTAINTY_ASSIGNED_CONTEXT((#10451))
GLOBAL_UNIT_ASSIGNED_CONTEXT((#10511,#10513,#10514))
REPRESENTATION_CONTEXT('','3D')
);
#10491=(
GEOMETRIC_REPRESENTATION_CONTEXT(3)
GLOBAL_UNCERTAINTY_ASSIGNED_CONTEXT((#10452))
GLOBAL_UNIT_ASSIGNED_CONTEXT((#10511,#10513,#10514))
REPRESENTATION_CONTEXT('','3D')
);
#10492=(
GEOMETRIC_REPRESENTATION_CONTEXT(3)
GLOBAL_UNCERTAINTY_ASSIGNED_CONTEXT((#10453))
GLOBAL_UNIT_ASSIGNED_CONTEXT((#10511,#10513,#10514))
REPRESENTATION_CONTEXT('','3D')
);
#10493=(
GEOMETRIC_REPRESENTATION_CONTEXT(3)
GLOBAL_UNCERTAINTY_ASSIGNED_CONTEXT((#10454))
GLOBAL_UNIT_ASSIGNED_CONTEXT((#10511,#10513,#10514))
REPRESENTATION_CONTEXT('','3D')
);
#10494=(
GEOMETRIC_REPRESENTATION_CONTEXT(3)
GLOBAL_UNCERTAINTY_ASSIGNED_CONTEXT((#10455))
GLOBAL_UNIT_ASSIGNED_CONTEXT((#10511,#10513,#10514))
REPRESENTATION_CONTEXT('','3D')
);
#10495=(
GEOMETRIC_REPRESENTATION_CONTEXT(3)
GLOBAL_UNCERTAINTY_ASSIGNED_CONTEXT((#10456))
GLOBAL_UNIT_ASSIGNED_CONTEXT((#10511,#10513,#10514))
REPRESENTATION_CONTEXT('','3D')
);
#10496=(
GEOMETRIC_REPRESENTATION_CONTEXT(3)
GLOBAL_UNCERTAINTY_ASSIGNED_CONTEXT((#10457))
GLOBAL_UNIT_ASSIGNED_CONTEXT((#10511,#10513,#10514))
REPRESENTATION_CONTEXT('','3D')
);
#10497=(
GEOMETRIC_REPRESENTATION_CONTEXT(3)
GLOBAL_UNCERTAINTY_ASSIGNED_CONTEXT((#10458))
GLOBAL_UNIT_ASSIGNED_CONTEXT((#10511,#10513,#10514))
REPRESENTATION_CONTEXT('','3D')
);
#10498=(
GEOMETRIC_REPRESENTATION_CONTEXT(3)
GLOBAL_UNCERTAINTY_ASSIGNED_CONTEXT((#10459))
GLOBAL_UNIT_ASSIGNED_CONTEXT((#10511,#10513,#10514))
REPRESENTATION_CONTEXT('','3D')
);
#10499=(
GEOMETRIC_REPRESENTATION_CONTEXT(3)
GLOBAL_UNCERTAINTY_ASSIGNED_CONTEXT((#10460))
GLOBAL_UNIT_ASSIGNED_CONTEXT((#10511,#10513,#10514))
REPRESENTATION_CONTEXT('','3D')
);
#10500=(
GEOMETRIC_REPRESENTATION_CONTEXT(3)
GLOBAL_UNCERTAINTY_ASSIGNED_CONTEXT((#10461))
GLOBAL_UNIT_ASSIGNED_CONTEXT((#10511,#10513,#10514))
REPRESENTATION_CONTEXT('','3D')
);
#10501=(
GEOMETRIC_REPRESENTATION_CONTEXT(3)
GLOBAL_UNCERTAINTY_ASSIGNED_CONTEXT((#10462))
GLOBAL_UNIT_ASSIGNED_CONTEXT((#10511,#10513,#10514))
REPRESENTATION_CONTEXT('','3D')
);
#10502=(
GEOMETRIC_REPRESENTATION_CONTEXT(3)
GLOBAL_UNCERTAINTY_ASSIGNED_CONTEXT((#10463))
GLOBAL_UNIT_ASSIGNED_CONTEXT((#10511,#10513,#10514))
REPRESENTATION_CONTEXT('','3D')
);
#10503=(
GEOMETRIC_REPRESENTATION_CONTEXT(3)
GLOBAL_UNCERTAINTY_ASSIGNED_CONTEXT((#10464))
GLOBAL_UNIT_ASSIGNED_CONTEXT((#10511,#10513,#10514))
REPRESENTATION_CONTEXT('','3D')
);
#10504=(
GEOMETRIC_REPRESENTATION_CONTEXT(3)
GLOBAL_UNCERTAINTY_ASSIGNED_CONTEXT((#10465))
GLOBAL_UNIT_ASSIGNED_CONTEXT((#10511,#10513,#10514))
REPRESENTATION_CONTEXT('','3D')
);
#10505=(
GEOMETRIC_REPRESENTATION_CONTEXT(3)
GLOBAL_UNCERTAINTY_ASSIGNED_CONTEXT((#10466))
GLOBAL_UNIT_ASSIGNED_CONTEXT((#10511,#10513,#10514))
REPRESENTATION_CONTEXT('','3D')
);
#10506=(
GEOMETRIC_REPRESENTATION_CONTEXT(3)
GLOBAL_UNCERTAINTY_ASSIGNED_CONTEXT((#10467))
GLOBAL_UNIT_ASSIGNED_CONTEXT((#10511,#10513,#10514))
REPRESENTATION_CONTEXT('','3D')
);
#10507=(
GEOMETRIC_REPRESENTATION_CONTEXT(3)
GLOBAL_UNCERTAINTY_ASSIGNED_CONTEXT((#10468))
GLOBAL_UNIT_ASSIGNED_CONTEXT((#10511,#10513,#10514))
REPRESENTATION_CONTEXT('','3D')
);
#10508=(
GEOMETRIC_REPRESENTATION_CONTEXT(3)
GLOBAL_UNCERTAINTY_ASSIGNED_CONTEXT((#10469))
GLOBAL_UNIT_ASSIGNED_CONTEXT((#10511,#10513,#10514))
REPRESENTATION_CONTEXT('','3D')
);
#10509=(
GEOMETRIC_REPRESENTATION_CONTEXT(3)
GLOBAL_UNCERTAINTY_ASSIGNED_CONTEXT((#10470))
GLOBAL_UNIT_ASSIGNED_CONTEXT((#10511,#10513,#10514))
REPRESENTATION_CONTEXT('','3D')
);
#10510=(
GEOMETRIC_REPRESENTATION_CONTEXT(3)
GLOBAL_UNCERTAINTY_ASSIGNED_CONTEXT((#10471))
GLOBAL_UNIT_ASSIGNED_CONTEXT((#10511,#10513,#10514))
REPRESENTATION_CONTEXT('','3D')
);
#10511=(
LENGTH_UNIT()
NAMED_UNIT(*)
SI_UNIT(.CENTI.,.METRE.)
);
#10512=(
LENGTH_UNIT()
NAMED_UNIT(*)
SI_UNIT($,.METRE.)
);
#10513=(
NAMED_UNIT(*)
PLANE_ANGLE_UNIT()
SI_UNIT($,.RADIAN.)
);
#10514=(
NAMED_UNIT(*)
SI_UNIT($,.STERADIAN.)
SOLID_ANGLE_UNIT()
);
#10515=SHAPE_DEFINITION_REPRESENTATION(#10553,#10645);
#10516=SHAPE_DEFINITION_REPRESENTATION(#10554,#10646);
#10517=SHAPE_DEFINITION_REPRESENTATION(#10555,#10647);
#10518=SHAPE_DEFINITION_REPRESENTATION(#10556,#10648);
#10519=SHAPE_DEFINITION_REPRESENTATION(#10557,#10649);
#10520=SHAPE_DEFINITION_REPRESENTATION(#10558,#10650);
#10521=SHAPE_DEFINITION_REPRESENTATION(#10559,#10651);
#10522=SHAPE_DEFINITION_REPRESENTATION(#10560,#10652);
#10523=SHAPE_DEFINITION_REPRESENTATION(#10561,#10653);
#10524=SHAPE_DEFINITION_REPRESENTATION(#10562,#10654);
#10525=SHAPE_DEFINITION_REPRESENTATION(#10563,#10655);
#10526=SHAPE_DEFINITION_REPRESENTATION(#10564,#10656);
#10527=SHAPE_DEFINITION_REPRESENTATION(#10565,#10657);
#10528=SHAPE_DEFINITION_REPRESENTATION(#10566,#10658);
#10529=SHAPE_DEFINITION_REPRESENTATION(#10567,#10659);
#10530=SHAPE_DEFINITION_REPRESENTATION(#10568,#10660);
#10531=SHAPE_DEFINITION_REPRESENTATION(#10569,#10661);
#10532=SHAPE_DEFINITION_REPRESENTATION(#10575,#10662);
#10533=SHAPE_DEFINITION_REPRESENTATION(#10576,#10663);
#10534=SHAPE_DEFINITION_REPRESENTATION(#10577,#10664);
#10535=SHAPE_DEFINITION_REPRESENTATION(#10578,#10665);
#10536=SHAPE_DEFINITION_REPRESENTATION(#10579,#10666);
#10537=SHAPE_DEFINITION_REPRESENTATION(#10580,#10667);
#10538=SHAPE_DEFINITION_REPRESENTATION(#10581,#10668);
#10539=SHAPE_DEFINITION_REPRESENTATION(#10582,#10669);
#10540=SHAPE_DEFINITION_REPRESENTATION(#10583,#10670);
#10541=SHAPE_DEFINITION_REPRESENTATION(#10584,#10671);
#10542=SHAPE_DEFINITION_REPRESENTATION(#10585,#10672);
#10543=SHAPE_DEFINITION_REPRESENTATION(#10586,#10673);
#10544=SHAPE_DEFINITION_REPRESENTATION(#10587,#10674);
#10545=SHAPE_DEFINITION_REPRESENTATION(#10588,#10675);
#10546=SHAPE_DEFINITION_REPRESENTATION(#10589,#10676);
#10547=SHAPE_DEFINITION_REPRESENTATION(#10590,#10677);
#10548=SHAPE_DEFINITION_REPRESENTATION(#10591,#10678);
#10549=SHAPE_DEFINITION_REPRESENTATION(#10597,#10679);
#10550=SHAPE_DEFINITION_REPRESENTATION(#10637,#10680);
#10551=SHAPE_DEFINITION_REPRESENTATION(#10638,#10681);
#10552=SHAPE_DEFINITION_REPRESENTATION(#10639,#10682);
#10553=PRODUCT_DEFINITION_SHAPE('',$,#10684);
#10554=PRODUCT_DEFINITION_SHAPE('',$,#10685);
#10555=PRODUCT_DEFINITION_SHAPE('',$,#10686);
#10556=PRODUCT_DEFINITION_SHAPE('',$,#10687);
#10557=PRODUCT_DEFINITION_SHAPE('',$,#10688);
#10558=PRODUCT_DEFINITION_SHAPE('',$,#10689);
#10559=PRODUCT_DEFINITION_SHAPE('',$,#10690);
#10560=PRODUCT_DEFINITION_SHAPE('',$,#10691);
#10561=PRODUCT_DEFINITION_SHAPE('',$,#10692);
#10562=PRODUCT_DEFINITION_SHAPE('',$,#10693);
#10563=PRODUCT_DEFINITION_SHAPE('',$,#10694);
#10564=PRODUCT_DEFINITION_SHAPE('',$,#10695);
#10565=PRODUCT_DEFINITION_SHAPE('',$,#10696);
#10566=PRODUCT_DEFINITION_SHAPE('',$,#10697);
#10567=PRODUCT_DEFINITION_SHAPE('',$,#10698);
#10568=PRODUCT_DEFINITION_SHAPE('',$,#10699);
#10569=PRODUCT_DEFINITION_SHAPE('',$,#10700);
#10570=PRODUCT_DEFINITION_SHAPE($,$,#173);
#10571=PRODUCT_DEFINITION_SHAPE($,$,#174);
#10572=PRODUCT_DEFINITION_SHAPE($,$,#175);
#10573=PRODUCT_DEFINITION_SHAPE($,$,#176);
#10574=PRODUCT_DEFINITION_SHAPE($,$,#177);
#10575=PRODUCT_DEFINITION_SHAPE('',$,#10701);
#10576=PRODUCT_DEFINITION_SHAPE('',$,#10702);
#10577=PRODUCT_DEFINITION_SHAPE('',$,#10703);
#10578=PRODUCT_DEFINITION_SHAPE('',$,#10704);
#10579=PRODUCT_DEFINITION_SHAPE('',$,#10705);
#10580=PRODUCT_DEFINITION_SHAPE('',$,#10706);
#10581=PRODUCT_DEFINITION_SHAPE('',$,#10707);
#10582=PRODUCT_DEFINITION_SHAPE('',$,#10708);
#10583=PRODUCT_DEFINITION_SHAPE('',$,#10709);
#10584=PRODUCT_DEFINITION_SHAPE('',$,#10710);
#10585=PRODUCT_DEFINITION_SHAPE('',$,#10711);
#10586=PRODUCT_DEFINITION_SHAPE('',$,#10712);
#10587=PRODUCT_DEFINITION_SHAPE('',$,#10713);
#10588=PRODUCT_DEFINITION_SHAPE('',$,#10714);
#10589=PRODUCT_DEFINITION_SHAPE('',$,#10715);
#10590=PRODUCT_DEFINITION_SHAPE('',$,#10716);
#10591=PRODUCT_DEFINITION_SHAPE('',$,#10717);
#10592=PRODUCT_DEFINITION_SHAPE($,$,#178);
#10593=PRODUCT_DEFINITION_SHAPE($,$,#179);
#10594=PRODUCT_DEFINITION_SHAPE($,$,#180);
#10595=PRODUCT_DEFINITION_SHAPE($,$,#181);
#10596=PRODUCT_DEFINITION_SHAPE($,$,#182);
#10597=PRODUCT_DEFINITION_SHAPE('',$,#10718);
#10598=PRODUCT_DEFINITION_SHAPE($,$,#183);
#10599=PRODUCT_DEFINITION_SHAPE($,$,#184);
#10600=PRODUCT_DEFINITION_SHAPE($,$,#185);
#10601=PRODUCT_DEFINITION_SHAPE($,$,#186);
#10602=PRODUCT_DEFINITION_SHAPE($,$,#187);
#10603=PRODUCT_DEFINITION_SHAPE($,$,#188);
#10604=PRODUCT_DEFINITION_SHAPE($,$,#189);
#10605=PRODUCT_DEFINITION_SHAPE($,$,#190);
#10606=PRODUCT_DEFINITION_SHAPE($,$,#191);
#10607=PRODUCT_DEFINITION_SHAPE($,$,#192);
#10608=PRODUCT_DEFINITION_SHAPE($,$,#193);
#10609=PRODUCT_DEFINITION_SHAPE($,$,#194);
#10610=PRODUCT_DEFINITION_SHAPE($,$,#195);
#10611=PRODUCT_DEFINITION_SHAPE($,$,#196);
#10612=PRODUCT_DEFINITION_SHAPE($,$,#197);
#10613=PRODUCT_DEFINITION_SHAPE($,$,#198);
#10614=PRODUCT_DEFINITION_SHAPE($,$,#199);
#10615=PRODUCT_DEFINITION_SHAPE($,$,#200);
#10616=PRODUCT_DEFINITION_SHAPE($,$,#201);
#10617=PRODUCT_DEFINITION_SHAPE($,$,#202);
#10618=PRODUCT_DEFINITION_SHAPE($,$,#203);
#10619=PRODUCT_DEFINITION_SHAPE($,$,#204);
#10620=PRODUCT_DEFINITION_SHAPE($,$,#205);
#10621=PRODUCT_DEFINITION_SHAPE($,$,#206);
#10622=PRODUCT_DEFINITION_SHAPE($,$,#207);
#10623=PRODUCT_DEFINITION_SHAPE($,$,#208);
#10624=PRODUCT_DEFINITION_SHAPE($,$,#209);
#10625=PRODUCT_DEFINITION_SHAPE($,$,#210);
#10626=PRODUCT_DEFINITION_SHAPE($,$,#211);
#10627=PRODUCT_DEFINITION_SHAPE($,$,#212);
#10628=PRODUCT_DEFINITION_SHAPE($,$,#213);
#10629=PRODUCT_DEFINITION_SHAPE($,$,#214);
#10630=PRODUCT_DEFINITION_SHAPE($,$,#215);
#10631=PRODUCT_DEFINITION_SHAPE($,$,#216);
#10632=PRODUCT_DEFINITION_SHAPE($,$,#217);
#10633=PRODUCT_DEFINITION_SHAPE($,$,#218);
#10634=PRODUCT_DEFINITION_SHAPE($,$,#219);
#10635=PRODUCT_DEFINITION_SHAPE($,$,#220);
#10636=PRODUCT_DEFINITION_SHAPE($,$,#221);
#10637=PRODUCT_DEFINITION_SHAPE('',$,#10719);
#10638=PRODUCT_DEFINITION_SHAPE('',$,#10720);
#10639=PRODUCT_DEFINITION_SHAPE('',$,#10721);
#10640=PRODUCT_DEFINITION_SHAPE($,$,#222);
#10641=PRODUCT_DEFINITION_SHAPE($,$,#223);
#10642=PRODUCT_DEFINITION_SHAPE($,$,#224);
#10643=PRODUCT_DEFINITION_SHAPE($,$,#225);
#10644=PRODUCT_DEFINITION_SHAPE($,$,#226);
#10645=SHAPE_REPRESENTATION('',(#5697,#6416,#6417,#6418),#10472);
#10646=SHAPE_REPRESENTATION('',(#5698,#6352,#6353,#6354,#6355,#6356,#6357,
#6358,#6359,#6360,#6361,#6362,#6363,#6364,#6365,#6366,#6367,#6368,#6369,
#6370,#6371,#6372,#6373,#6374,#6375,#6376),#10473);
#10647=SHAPE_REPRESENTATION('',(#5699),#10474);
#10648=SHAPE_REPRESENTATION('',(#5718),#10475);
#10649=SHAPE_REPRESENTATION('',(#5725),#10476);
#10650=SHAPE_REPRESENTATION('',(#5732),#10477);
#10651=SHAPE_REPRESENTATION('',(#5770),#10478);
#10652=SHAPE_REPRESENTATION('',(#5779),#10479);
#10653=SHAPE_REPRESENTATION('',(#5804),#10480);
#10654=SHAPE_REPRESENTATION('',(#5829),#10481);
#10655=SHAPE_REPRESENTATION('',(#5838),#10482);
#10656=SHAPE_REPRESENTATION('',(#5862,#5985,#5986,#5987,#5988,#5989),#10483);
#10657=SHAPE_REPRESENTATION('',(#5863),#10484);
#10658=SHAPE_REPRESENTATION('',(#5883),#10485);
#10659=SHAPE_REPRESENTATION('',(#5903),#10486);
#10660=SHAPE_REPRESENTATION('',(#5918),#10487);
#10661=SHAPE_REPRESENTATION('',(#5968),#10488);
#10662=SHAPE_REPRESENTATION('',(#5990,#6377,#6378,#6379,#6380,#6381,#6382,
#6383,#6384,#6385,#6386,#6387,#6388,#6389,#6390),#10489);
#10663=SHAPE_REPRESENTATION('',(#5991),#10490);
#10664=SHAPE_REPRESENTATION('',(#6012),#10491);
#10665=SHAPE_REPRESENTATION('',(#6062),#10492);
#10666=SHAPE_REPRESENTATION('',(#6071),#10493);
#10667=SHAPE_REPRESENTATION('',(#6086),#10494);
#10668=SHAPE_REPRESENTATION('',(#6110),#10495);
#10669=SHAPE_REPRESENTATION('',(#6119),#10496);
#10670=SHAPE_REPRESENTATION('',(#6128),#10497);
#10671=SHAPE_REPRESENTATION('',(#6151),#10498);
#10672=SHAPE_REPRESENTATION('',(#6168),#10499);
#10673=SHAPE_REPRESENTATION('',(#6192,#6321,#6322,#6323,#6324,#6325),#10500);
#10674=SHAPE_REPRESENTATION('',(#6193),#10501);
#10675=SHAPE_REPRESENTATION('',(#6213),#10502);
#10676=SHAPE_REPRESENTATION('',(#6233),#10503);
#10677=SHAPE_REPRESENTATION('',(#6250),#10504);
#10678=SHAPE_REPRESENTATION('',(#6304),#10505);
#10679=SHAPE_REPRESENTATION('',(#6326),#10506);
#10680=SHAPE_REPRESENTATION('',(#6391,#6414,#6415),#10507);
#10681=SHAPE_REPRESENTATION('',(#6392),#10508);
#10682=SHAPE_REPRESENTATION('',(#6405),#10509);
#10683=PRODUCT_DEFINITION_CONTEXT('part definition',#10799,'design');
#10684=PRODUCT_DEFINITION('PAT-050',
'PAT-050',#10722,#10683);
#10685=PRODUCT_DEFINITION('Bearing stand','Bearing stand',#10723,#10683);
#10686=PRODUCT_DEFINITION('Base','Base',#10724,#10683);
#10687=PRODUCT_DEFINITION('Bonded pad','Bonded pad',#10725,#10683);
#10688=PRODUCT_DEFINITION('Bonded pad (1)','Bonded pad (1)',#10726,#10683);
#10689=PRODUCT_DEFINITION('Bearing pedestal','Bearing pedestal',#10727,
#10683);
#10690=PRODUCT_DEFINITION('Outer race spacer','Outer race spacer',#10728,
#10683);
#10691=PRODUCT_DEFINITION('Bearing cap','Bearing cap',#10729,#10683);
#10692=PRODUCT_DEFINITION('Bearing cap (1)','Bearing cap (1)',#10730,#10683);
#10693=PRODUCT_DEFINITION('Flat Washer - M6','Flat Washer - M6',#10731,
#10683);
#10694=PRODUCT_DEFINITION('M6x18 mounting screw','M6x18 mounting screw',
#10732,#10683);
#10695=PRODUCT_DEFINITION('Sealed Ball Bearing - 12 x 32 x 10 mm',
'Sealed Ball Bearing - 12 x 32 x 10 mm',#10733,#10683);
#10696=PRODUCT_DEFINITION('Inner ring','Inner ring',#10734,#10683);
#10697=PRODUCT_DEFINITION('Outer ring','Outer ring',#10735,#10683);
#10698=PRODUCT_DEFINITION('Balls','Balls',#10736,#10683);
#10699=PRODUCT_DEFINITION('Cage','Cage',#10737,#10683);
#10700=PRODUCT_DEFINITION('Seals 2RS','Seals 2RS',#10738,#10683);
#10701=PRODUCT_DEFINITION('Wheel and shaft','Wheel and shaft',#10739,#10683);
#10702=PRODUCT_DEFINITION('Shaft','Shaft',#10740,#10683);
#10703=PRODUCT_DEFINITION('Hand wheel','Hand wheel',#10741,#10683);
#10704=PRODUCT_DEFINITION('Inner race spacer','Inner race spacer',#10742,
#10683);
#10705=PRODUCT_DEFINITION('Shaft collar','Shaft collar',#10743,#10683);
#10706=PRODUCT_DEFINITION('Handle axle','Handle axle',#10744,#10683);
#10707=PRODUCT_DEFINITION('Handle inner spacer','Handle inner spacer',#10745,
#10683);
#10708=PRODUCT_DEFINITION('Handle axle keeper','Handle axle keeper',#10746,
#10683);
#10709=PRODUCT_DEFINITION('Parallel Key - 4x4x20',
'Parallel Key - 4x4x20',#10747,#10683);
#10710=PRODUCT_DEFINITION('Socket Set Screw - M5x8',
'Socket Set Screw - M5x8',#10748,#10683);
#10711=PRODUCT_DEFINITION('M4x10 handle screw','M4x10 handle screw',#10749,
#10683);
#10712=PRODUCT_DEFINITION('Sealed Ball Bearing - 10 x 30 x 9 mm',
'Sealed Ball Bearing - 10 x 30 x 9 mm',#10750,#10683);
#10713=PRODUCT_DEFINITION('Inner ring (1)','Inner ring (1)',#10751,#10683);
#10714=PRODUCT_DEFINITION('Outer ring (1)','Outer ring (1)',#10752,#10683);
#10715=PRODUCT_DEFINITION('Balls (1)','Balls (1)',#10753,#10683);
#10716=PRODUCT_DEFINITION('Cage (1)','Cage (1)',#10754,#10683);
#10717=PRODUCT_DEFINITION('Seals 2RS (1)','Seals 2RS (1)',#10755,#10683);
#10718=PRODUCT_DEFINITION('Cap Screw - M4x16','Cap Screw - M4x16',#10756,
#10683);
#10719=PRODUCT_DEFINITION('Revolving handle','Revolving handle',#10757,
#10683);
#10720=PRODUCT_DEFINITION('Revolving grip','Revolving grip',#10758,#10683);
#10721=PRODUCT_DEFINITION('Grip bearing cap','Grip bearing cap',#10759,
#10683);
#10722=PRODUCT_DEFINITION_FORMATION('',$,#10801);
#10723=PRODUCT_DEFINITION_FORMATION('',$,#10802);
#10724=PRODUCT_DEFINITION_FORMATION('',$,#10803);
#10725=PRODUCT_DEFINITION_FORMATION('',$,#10804);
#10726=PRODUCT_DEFINITION_FORMATION('',$,#10805);
#10727=PRODUCT_DEFINITION_FORMATION('',$,#10806);
#10728=PRODUCT_DEFINITION_FORMATION('',$,#10807);
#10729=PRODUCT_DEFINITION_FORMATION('',$,#10808);
#10730=PRODUCT_DEFINITION_FORMATION('',$,#10809);
#10731=PRODUCT_DEFINITION_FORMATION('',$,#10810);
#10732=PRODUCT_DEFINITION_FORMATION('',$,#10811);
#10733=PRODUCT_DEFINITION_FORMATION('',$,#10812);
#10734=PRODUCT_DEFINITION_FORMATION('',$,#10813);
#10735=PRODUCT_DEFINITION_FORMATION('',$,#10814);
#10736=PRODUCT_DEFINITION_FORMATION('',$,#10815);
#10737=PRODUCT_DEFINITION_FORMATION('',$,#10816);
#10738=PRODUCT_DEFINITION_FORMATION('',$,#10817);
#10739=PRODUCT_DEFINITION_FORMATION('',$,#10818);
#10740=PRODUCT_DEFINITION_FORMATION('',$,#10819);
#10741=PRODUCT_DEFINITION_FORMATION('',$,#10820);
#10742=PRODUCT_DEFINITION_FORMATION('',$,#10821);
#10743=PRODUCT_DEFINITION_FORMATION('',$,#10822);
#10744=PRODUCT_DEFINITION_FORMATION('',$,#10823);
#10745=PRODUCT_DEFINITION_FORMATION('',$,#10824);
#10746=PRODUCT_DEFINITION_FORMATION('',$,#10825);
#10747=PRODUCT_DEFINITION_FORMATION('',$,#10826);
#10748=PRODUCT_DEFINITION_FORMATION('',$,#10827);
#10749=PRODUCT_DEFINITION_FORMATION('',$,#10828);
#10750=PRODUCT_DEFINITION_FORMATION('',$,#10829);
#10751=PRODUCT_DEFINITION_FORMATION('',$,#10830);
#10752=PRODUCT_DEFINITION_FORMATION('',$,#10831);
#10753=PRODUCT_DEFINITION_FORMATION('',$,#10832);
#10754=PRODUCT_DEFINITION_FORMATION('',$,#10833);
#10755=PRODUCT_DEFINITION_FORMATION('',$,#10834);
#10756=PRODUCT_DEFINITION_FORMATION('',$,#10835);
#10757=PRODUCT_DEFINITION_FORMATION('',$,#10836);
#10758=PRODUCT_DEFINITION_FORMATION('',$,#10837);
#10759=PRODUCT_DEFINITION_FORMATION('',$,#10838);
#10760=PRODUCT_RELATED_PRODUCT_CATEGORY('PAT-050','PAT-050',(#10801));
#10761=PRODUCT_RELATED_PRODUCT_CATEGORY('Bearing stand','Bearing stand',
(#10802));
#10762=PRODUCT_RELATED_PRODUCT_CATEGORY('Base','Base',(#10803));
#10763=PRODUCT_RELATED_PRODUCT_CATEGORY('Bonded pad','Bonded pad',(#10804));
#10764=PRODUCT_RELATED_PRODUCT_CATEGORY('Bonded pad (1)',
'Bonded pad (1)',(#10805));
#10765=PRODUCT_RELATED_PRODUCT_CATEGORY('Bearing pedestal',
'Bearing pedestal',(#10806));
#10766=PRODUCT_RELATED_PRODUCT_CATEGORY('Outer race spacer',
'Outer race spacer',(#10807));
#10767=PRODUCT_RELATED_PRODUCT_CATEGORY('Bearing cap','Bearing cap',(#10808));
#10768=PRODUCT_RELATED_PRODUCT_CATEGORY('Bearing cap (1)',
'Bearing cap (1)',(#10809));
#10769=PRODUCT_RELATED_PRODUCT_CATEGORY('Flat Washer - M6',
'Flat Washer - M6',(#10810));
#10770=PRODUCT_RELATED_PRODUCT_CATEGORY('M6x18 mounting screw',
'M6x18 mounting screw',(#10811));
#10771=PRODUCT_RELATED_PRODUCT_CATEGORY(
'Sealed Ball Bearing - 12 x 32 x 10 mm',
'Sealed Ball Bearing - 12 x 32 x 10 mm',(#10812));
#10772=PRODUCT_RELATED_PRODUCT_CATEGORY('Inner ring','Inner ring',(#10813));
#10773=PRODUCT_RELATED_PRODUCT_CATEGORY('Outer ring','Outer ring',(#10814));
#10774=PRODUCT_RELATED_PRODUCT_CATEGORY('Balls','Balls',(#10815));
#10775=PRODUCT_RELATED_PRODUCT_CATEGORY('Cage','Cage',(#10816));
#10776=PRODUCT_RELATED_PRODUCT_CATEGORY('Seals 2RS','Seals 2RS',(#10817));
#10777=PRODUCT_RELATED_PRODUCT_CATEGORY('Wheel and shaft',
'Wheel and shaft',(#10818));
#10778=PRODUCT_RELATED_PRODUCT_CATEGORY('Shaft','Shaft',(#10819));
#10779=PRODUCT_RELATED_PRODUCT_CATEGORY('Hand wheel','Hand wheel',(#10820));
#10780=PRODUCT_RELATED_PRODUCT_CATEGORY('Inner race spacer',
'Inner race spacer',(#10821));
#10781=PRODUCT_RELATED_PRODUCT_CATEGORY('Shaft collar','Shaft collar',(#10822));
#10782=PRODUCT_RELATED_PRODUCT_CATEGORY('Handle axle','Handle axle',(#10823));
#10783=PRODUCT_RELATED_PRODUCT_CATEGORY('Handle inner spacer',
'Handle inner spacer',(#10824));
#10784=PRODUCT_RELATED_PRODUCT_CATEGORY('Handle axle keeper',
'Handle axle keeper',(#10825));
#10785=PRODUCT_RELATED_PRODUCT_CATEGORY('Parallel Key - 4x4x20',
'Parallel Key - 4x4x20',(#10826));
#10786=PRODUCT_RELATED_PRODUCT_CATEGORY('Socket Set Screw - M5x8',
'Socket Set Screw - M5x8',(#10827));
#10787=PRODUCT_RELATED_PRODUCT_CATEGORY('M4x10 handle screw',
'M4x10 handle screw',(#10828));
#10788=PRODUCT_RELATED_PRODUCT_CATEGORY(
'Sealed Ball Bearing - 10 x 30 x 9 mm',
'Sealed Ball Bearing - 10 x 30 x 9 mm',(#10829));
#10789=PRODUCT_RELATED_PRODUCT_CATEGORY('Inner ring (1)',
'Inner ring (1)',(#10830));
#10790=PRODUCT_RELATED_PRODUCT_CATEGORY('Outer ring (1)',
'Outer ring (1)',(#10831));
#10791=PRODUCT_RELATED_PRODUCT_CATEGORY('Balls (1)','Balls (1)',(#10832));
#10792=PRODUCT_RELATED_PRODUCT_CATEGORY('Cage (1)','Cage (1)',(#10833));
#10793=PRODUCT_RELATED_PRODUCT_CATEGORY('Seals 2RS (1)','Seals 2RS (1)',
(#10834));
#10794=PRODUCT_RELATED_PRODUCT_CATEGORY('Cap Screw - M4x16',
'Cap Screw - M4x16',(#10835));
#10795=PRODUCT_RELATED_PRODUCT_CATEGORY('Revolving handle',
'Revolving handle',(#10836));
#10796=PRODUCT_RELATED_PRODUCT_CATEGORY('Revolving grip',
'Revolving grip',(#10837));
#10797=PRODUCT_RELATED_PRODUCT_CATEGORY('Grip bearing cap',
'Grip bearing cap',(#10838));
#10798=APPLICATION_PROTOCOL_DEFINITION('international standard',
'automotive_design',2009,#10799);
#10799=APPLICATION_CONTEXT(
'Core Data for Automotive Mechanical Design Process');
#10800=PRODUCT_CONTEXT('part definition',#10799,'mechanical');
#10801=PRODUCT('PAT-050','PAT-050',
'PAT-050',(#10800));
#10802=PRODUCT('Bearing stand','Bearing stand','Bearing stand',(#10800));
#10803=PRODUCT('Base','Base','Base',(#10800));
#10804=PRODUCT('Bonded pad','Bonded pad','Bonded pad',(#10800));
#10805=PRODUCT('Bonded pad (1)','Bonded pad (1)','Bonded pad (1)',(#10800));
#10806=PRODUCT('Bearing pedestal','Bearing pedestal','Bearing pedestal',
(#10800));
#10807=PRODUCT('Outer race spacer','Outer race spacer',
'Outer race spacer',(#10800));
#10808=PRODUCT('Bearing cap','Bearing cap','Bearing cap',(#10800));
#10809=PRODUCT('Bearing cap (1)','Bearing cap (1)','Bearing cap (1)',(#10800));
#10810=PRODUCT('Flat Washer - M6','Flat Washer - M6','Flat Washer - M6',
(#10800));
#10811=PRODUCT('M6x18 mounting screw','M6x18 mounting screw',
'M6x18 mounting screw',(#10800));
#10812=PRODUCT('Sealed Ball Bearing - 12 x 32 x 10 mm',
'Sealed Ball Bearing - 12 x 32 x 10 mm',
'Sealed Ball Bearing - 12 x 32 x 10 mm',(#10800));
#10813=PRODUCT('Inner ring','Inner ring','Inner ring',(#10800));
#10814=PRODUCT('Outer ring','Outer ring','Outer ring',(#10800));
#10815=PRODUCT('Balls','Balls','Balls',(#10800));
#10816=PRODUCT('Cage','Cage','Cage',(#10800));
#10817=PRODUCT('Seals 2RS','Seals 2RS','Seals 2RS',(#10800));
#10818=PRODUCT('Wheel and shaft','Wheel and shaft','Wheel and shaft',(#10800));
#10819=PRODUCT('Shaft','Shaft','Shaft',(#10800));
#10820=PRODUCT('Hand wheel','Hand wheel','Hand wheel',(#10800));
#10821=PRODUCT('Inner race spacer','Inner race spacer',
'Inner race spacer',(#10800));
#10822=PRODUCT('Shaft collar','Shaft collar','Shaft collar',(#10800));
#10823=PRODUCT('Handle axle','Handle axle','Handle axle',(#10800));
#10824=PRODUCT('Handle inner spacer','Handle inner spacer',
'Handle inner spacer',(#10800));
#10825=PRODUCT('Handle axle keeper','Handle axle keeper',
'Handle axle keeper',(#10800));
#10826=PRODUCT('Parallel Key - 4x4x20','Parallel Key - 4x4x20',
'Parallel Key - 4x4x20',(#10800));
#10827=PRODUCT('Socket Set Screw - M5x8','Socket Set Screw - M5x8',
'Socket Set Screw - M5x8',(#10800));
#10828=PRODUCT('M4x10 handle screw','M4x10 handle screw',
'M4x10 handle screw',(#10800));
#10829=PRODUCT('Sealed Ball Bearing - 10 x 30 x 9 mm',
'Sealed Ball Bearing - 10 x 30 x 9 mm',
'Sealed Ball Bearing - 10 x 30 x 9 mm',(#10800));
#10830=PRODUCT('Inner ring (1)','Inner ring (1)','Inner ring (1)',(#10800));
#10831=PRODUCT('Outer ring (1)','Outer ring (1)','Outer ring (1)',(#10800));
#10832=PRODUCT('Balls (1)','Balls (1)','Balls (1)',(#10800));
#10833=PRODUCT('Cage (1)','Cage (1)','Cage (1)',(#10800));
#10834=PRODUCT('Seals 2RS (1)','Seals 2RS (1)','Seals 2RS (1)',(#10800));
#10835=PRODUCT('Cap Screw - M4x16','Cap Screw - M4x16',
'Cap Screw - M4x16',(#10800));
#10836=PRODUCT('Revolving handle','Revolving handle','Revolving handle',
(#10800));
#10837=PRODUCT('Revolving grip','Revolving grip','Revolving grip',(#10800));
#10838=PRODUCT('Grip bearing cap','Grip bearing cap','Grip bearing cap',
(#10800));
#10839=PRESENTATION_STYLE_ASSIGNMENT((#10845));
#10840=PRESENTATION_STYLE_ASSIGNMENT((#10846));
#10841=PRESENTATION_STYLE_ASSIGNMENT((#10847));
#10842=PRESENTATION_STYLE_ASSIGNMENT((#10848));
#10843=PRESENTATION_STYLE_ASSIGNMENT((#10849));
#10844=PRESENTATION_STYLE_ASSIGNMENT((#10850));
#10845=SURFACE_STYLE_USAGE(.BOTH.,#10851);
#10846=SURFACE_STYLE_USAGE(.BOTH.,#10852);
#10847=SURFACE_STYLE_USAGE(.BOTH.,#10853);
#10848=SURFACE_STYLE_USAGE(.BOTH.,#10854);
#10849=SURFACE_STYLE_USAGE(.BOTH.,#10855);
#10850=SURFACE_STYLE_USAGE(.BOTH.,#10856);
#10851=SURFACE_SIDE_STYLE('',(#10857));
#10852=SURFACE_SIDE_STYLE('',(#10858));
#10853=SURFACE_SIDE_STYLE('',(#10859));
#10854=SURFACE_SIDE_STYLE('',(#10860));
#10855=SURFACE_SIDE_STYLE('',(#10861));
#10856=SURFACE_SIDE_STYLE('',(#10862));
#10857=SURFACE_STYLE_FILL_AREA(#10863);
#10858=SURFACE_STYLE_FILL_AREA(#10864);
#10859=SURFACE_STYLE_FILL_AREA(#10865);
#10860=SURFACE_STYLE_FILL_AREA(#10866);
#10861=SURFACE_STYLE_FILL_AREA(#10867);
#10862=SURFACE_STYLE_FILL_AREA(#10868);
#10863=FILL_AREA_STYLE('Steel - Satin',(#10869));
#10864=FILL_AREA_STYLE('CAD Library Painted - Deep blue',(#10870));
#10865=FILL_AREA_STYLE('CAD Library Painted - Graphite',(#10871));
#10866=FILL_AREA_STYLE('CAD Library Painted - Steel gray',(#10872));
#10867=FILL_AREA_STYLE('CAD Library Painted - Engineering blue',(#10873));
#10868=FILL_AREA_STYLE('CAD Library Painted - Light blue',(#10874));
#10869=FILL_AREA_STYLE_COLOUR('Steel - Satin',#10875);
#10870=FILL_AREA_STYLE_COLOUR('CAD Library Painted - Deep blue',#10876);
#10871=FILL_AREA_STYLE_COLOUR('CAD Library Painted - Graphite',#10877);
#10872=FILL_AREA_STYLE_COLOUR('CAD Library Painted - Steel gray',#10878);
#10873=FILL_AREA_STYLE_COLOUR('CAD Library Painted - Engineering blue',
#10879);
#10874=FILL_AREA_STYLE_COLOUR('CAD Library Painted - Light blue',#10880);
#10875=COLOUR_RGB('Steel - Satin',0.627450980392157,0.627450980392157,0.627450980392157);
#10876=COLOUR_RGB('CAD Library Painted - Deep blue',0.0784313725490196,
0.203921568627451,0.349019607843137);
#10877=COLOUR_RGB('CAD Library Painted - Graphite',0.168627450980392,0.192156862745098,
0.231372549019608);
#10878=COLOUR_RGB('CAD Library Painted - Steel gray',0.592156862745098,
0.631372549019608,0.67843137254902);
#10879=COLOUR_RGB('CAD Library Painted - Engineering blue',0.12156862745098,
0.356862745098039,0.6);
#10880=COLOUR_RGB('CAD Library Painted - Light blue',0.286274509803922,
0.552941176470588,0.780392156862745);
#10881=COLOUR_RGB('Dark Blue',0.08,0.2,0.34);
#10882=FILL_AREA_STYLE_COLOUR('',#10881);
#10883=FILL_AREA_STYLE('',(#10882));
#10884=SURFACE_STYLE_FILL_AREA(#10883);
#10885=SURFACE_SIDE_STYLE('',(#10884));
#10886=SURFACE_STYLE_USAGE(.BOTH.,#10885);
#10887=PRESENTATION_STYLE_ASSIGNMENT((#10886));
#10888=COLOUR_RGB('Light Blue',0.38,0.62,0.78);
#10889=FILL_AREA_STYLE_COLOUR('',#10888);
#10890=FILL_AREA_STYLE('',(#10889));
#10891=SURFACE_STYLE_FILL_AREA(#10890);
#10892=SURFACE_SIDE_STYLE('',(#10891));
#10893=SURFACE_STYLE_USAGE(.BOTH.,#10892);
#10894=PRESENTATION_STYLE_ASSIGNMENT((#10893));
#10895=COLOUR_RGB('Sky Blue',0.24,0.69,0.87);
#10896=FILL_AREA_STYLE_COLOUR('',#10895);
#10897=FILL_AREA_STYLE('',(#10896));
#10898=SURFACE_STYLE_FILL_AREA(#10897);
#10899=SURFACE_SIDE_STYLE('',(#10898));
#10900=SURFACE_STYLE_USAGE(.BOTH.,#10899);
#10901=PRESENTATION_STYLE_ASSIGNMENT((#10900));
#10902=COLOUR_RGB('Grey',0.48,0.52,0.57);
#10903=FILL_AREA_STYLE_COLOUR('',#10902);
#10904=FILL_AREA_STYLE('',(#10903));
#10905=SURFACE_STYLE_FILL_AREA(#10904);
#10906=SURFACE_SIDE_STYLE('',(#10905));
#10907=SURFACE_STYLE_USAGE(.BOTH.,#10906);
#10908=PRESENTATION_STYLE_ASSIGNMENT((#10907));
#10909=COLOUR_RGB('Black',0.12,0.14,0.17);
#10910=FILL_AREA_STYLE_COLOUR('',#10909);
#10911=FILL_AREA_STYLE('',(#10910));
#10912=SURFACE_STYLE_FILL_AREA(#10911);
#10913=SURFACE_SIDE_STYLE('',(#10912));
#10914=SURFACE_STYLE_USAGE(.BOTH.,#10913);
#10915=PRESENTATION_STYLE_ASSIGNMENT((#10914));
#10916=COLOUR_RGB('Off White',0.89,0.88,0.83);
#10917=FILL_AREA_STYLE_COLOUR('',#10916);
#10918=FILL_AREA_STYLE('',(#10917));
#10919=SURFACE_STYLE_FILL_AREA(#10918);
#10920=SURFACE_SIDE_STYLE('',(#10919));
#10921=SURFACE_STYLE_USAGE(.BOTH.,#10920);
#10922=PRESENTATION_STYLE_ASSIGNMENT((#10921));
ENDSEC;
END-ISO-10303-21;
